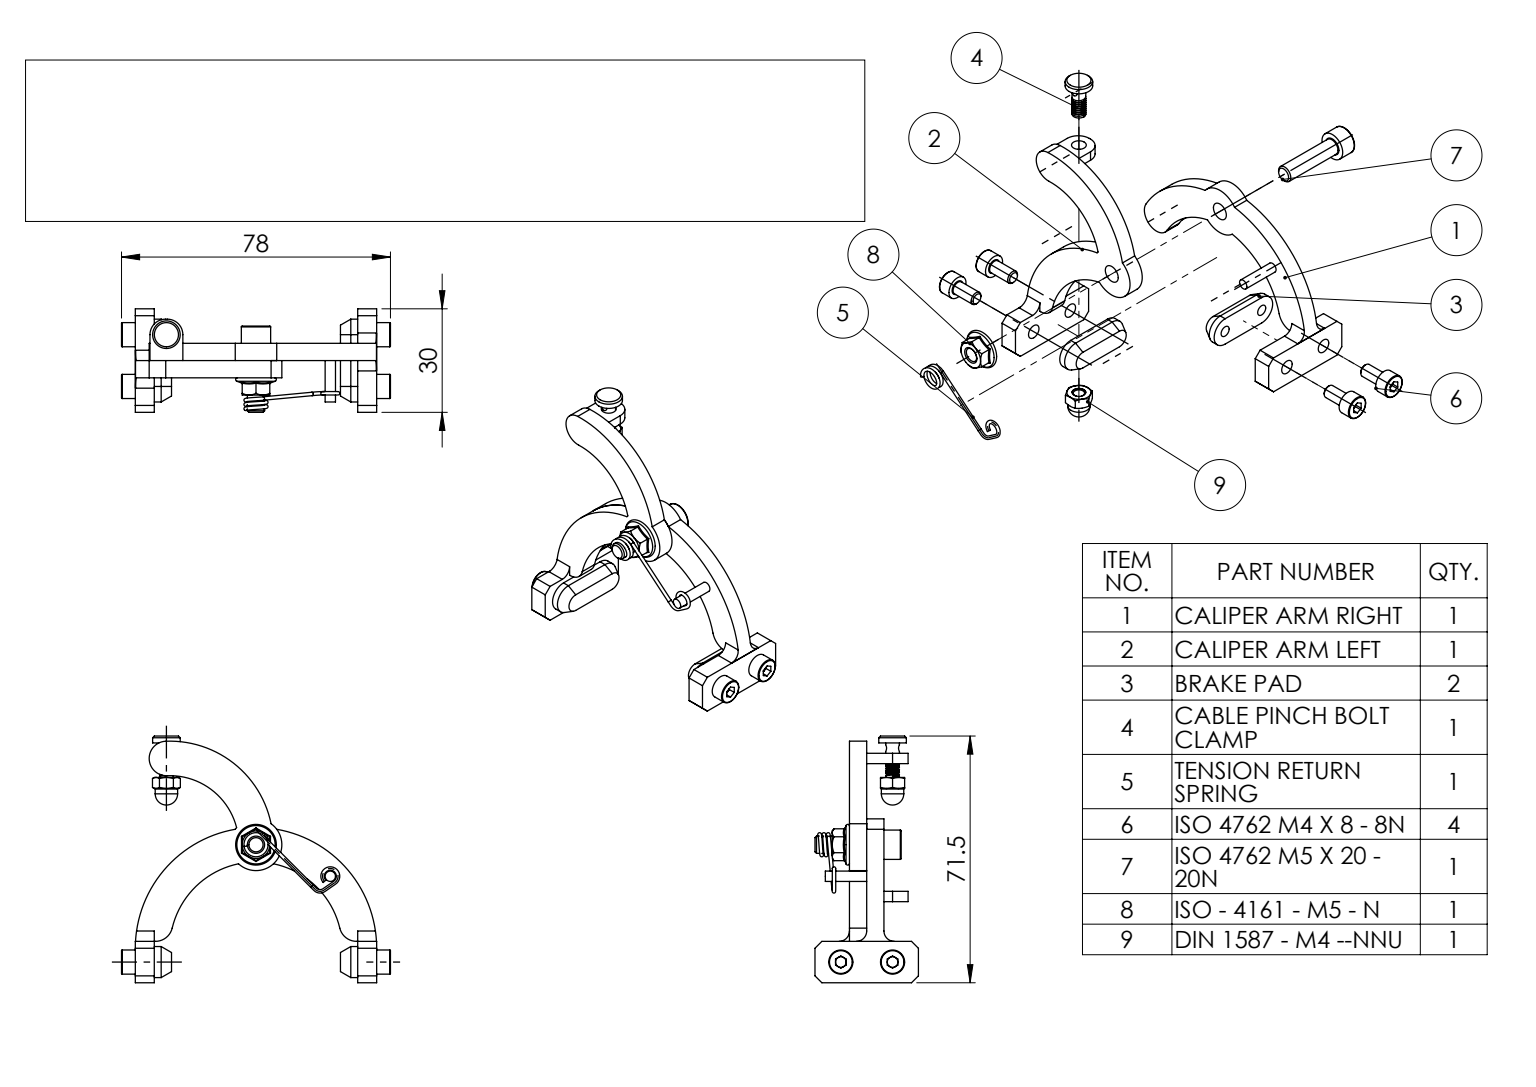
ISO-10303-21;
HEADER;
FILE_DESCRIPTION (('STEP AP214'),
    '1' );
FILE_NAME ('BR-590',
    '2026-10-08T05:45:04',
    ( '' ),
    ( '' ),
    'SwSTEP 2.0',
    'SolidWorks 2026',
    '' );
FILE_SCHEMA (( 'AUTOMOTIVE_DESIGN' ));
ENDSEC;

DATA;
#1 = CARTESIAN_POINT ( 'NONE',  ( 16.54959645279592451, 16.98593745313911896, 13.11591282735340336 ) ) ;
#2 =( LENGTH_UNIT ( ) NAMED_UNIT ( * ) SI_UNIT ( .MILLI., .METRE. ) );
#3 = CARTESIAN_POINT ( 'NONE',  ( 16.03488360228399046, 17.50065030364834939, 12.16198771834506509 ) ) ;
#4 = B_SPLINE_CURVE_WITH_KNOTS ( 'NONE', 3,
 ( #2921, #5637, #7133, #6355, #5528 ),
 .UNSPECIFIED., .F., .F.,
 ( 4, 1, 4 ),
 ( 5.640274452250024914E-20, 0.002309401076758505356, 0.004618802153517010713 ),
 .UNSPECIFIED. ) ;
#5 = CARTESIAN_POINT ( 'NONE',  ( 22.63806431670481700, 19.48506897666907989, 12.00579112326951758 ) ) ;
#6 = CARTESIAN_POINT ( 'NONE',  ( -25.98076211353311393, 52.34374999904395054, -3.128098921329806714 ) ) ;
#7 = CARTESIAN_POINT ( 'NONE',  ( -2.527408190673963162, 30.96936468028755840, 15.39281658473306358 ) ) ;
#8 = CARTESIAN_POINT ( 'NONE',  ( 3.200000000000000178, 2.020725942163657862, -3.499999999999999556 ) ) ;
#9 =( BOUNDED_CURVE ( )  B_SPLINE_CURVE ( 2, ( #10910, #4195, #7581, #6742, #4979, #7521, #70, #5149, #6620 ),
 .UNSPECIFIED., .F., .F. ) 
 B_SPLINE_CURVE_WITH_KNOTS ( ( 3, 2, 2, 2, 3 ),
 ( 0.6944444444444445308, 0.7037037037037037202, 0.7222222222222222099, 0.7407407407407406996, 0.7500000000000000000 ),
 .UNSPECIFIED. ) 
 CURVE ( )  GEOMETRIC_REPRESENTATION_ITEM ( )  RATIONAL_B_SPLINE_CURVE ( ( 0.9330127018922194093, 0.9330127018922197424, 1.000000000000000000, 0.8660254037844387076, 1.000000000000000000, 0.8660254037844387076, 1.000000000000000000, 0.9330127018922194093, 0.9330127018922194093 ) ) 
 REPRESENTATION_ITEM ( '' )  );
#10 = FACE_OUTER_BOUND ( 'NONE', #392, .T. ) ;
#11 = FACE_OUTER_BOUND ( 'NONE', #1428, .T. ) ;
#12 = VERTEX_POINT ( 'NONE', #2248 ) ;
#13 = ORIENTED_EDGE ( 'NONE', *, *, #10452, .T. ) ;
#14 = DIRECTION ( 'NONE',  ( 0.000000000000000000, 0.000000000000000000, 1.000000000000000000 ) ) ;
#15 = CONICAL_SURFACE ( 'NONE', #541, 4.000000000000000000, 0.8911886515913786111 ) ;
#16 = CARTESIAN_POINT ( 'NONE',  ( -4.211405944401398038, -2.460460786169389902, -3.751298493805494072 ) ) ;
#17 = CARTESIAN_POINT ( 'NONE',  ( 19.95755123817951215, 17.62047157401400810, 12.00579112326941988 ) ) ;
#18 = UNCERTAINTY_MEASURE_WITH_UNIT (LENGTH_MEASURE( 1.000000000000000082E-05 ), #5479, 'distance_accuracy_value', 'NONE');
#19 = CARTESIAN_POINT ( 'NONE',  ( -2.500000000000005329, 29.80321974748362734, 16.48359592357600789 ) ) ;
#20 = EDGE_CURVE ( 'NONE', #10326, #5059, #2301, .T. ) ;
#21 = LINE ( 'NONE', #8698, #9426 ) ;
#22 = CARTESIAN_POINT ( 'NONE',  ( -24.35964822603314417, 53.91874999904395338, -5.000000000000103029 ) ) ;
#23 = ADVANCED_FACE ( 'NONE', ( #9179, #3240, #3960 ), #10018, .T. ) ;
#24 = LINE ( 'NONE', #3426, #7602 ) ;
#25 = FACE_OUTER_BOUND ( 'NONE', #10724, .T. ) ;
#26 = CARTESIAN_POINT ( 'NONE',  ( 4.750000000000000888, 3.249999999999998668, 0.000000000000000000 ) ) ;
#27 = VECTOR ( 'NONE', #4855, 1000.000000000000000 ) ;
#28 = ORIENTED_EDGE ( 'NONE', *, *, #6003, .T. ) ;
#29 = DIRECTION ( 'NONE',  ( 6.098637220230963674E-17, -1.000000000000000000, 0.000000000000000000 ) ) ;
#30 = CARTESIAN_POINT ( 'NONE',  ( -25.98076211353311038, 60.99999999999985789, -0.9999999999995021760 ) ) ;
#31 = CARTESIAN_POINT ( 'NONE',  ( -24.35964822603314772, 52.63541666571061484, -4.064049460664953983 ) ) ;
#32 = CARTESIAN_POINT ( 'NONE',  ( -24.35964822603314772, 55.26041666571061484, -4.064049460664953983 ) ) ;
#33 = ADVANCED_FACE ( 'NONE', ( #727 ), #6680, .T. ) ;
#34 = CARTESIAN_POINT ( 'NONE',  ( 5.076455387921347651, 24.47916666666666075, -2.499999999999999112 ) ) ;
#35 = CARTESIAN_POINT ( 'NONE',  ( -26.98076211353309972, 53.23333333333319217, -6.732050807568954909 ) ) ;
#36 = AXIS2_PLACEMENT_3D ( 'NONE', #5242, #7853, #1848 ) ;
#37 = ORIENTED_EDGE ( 'NONE', *, *, #2342, .T. ) ;
#38 = VERTEX_POINT ( 'NONE', #5852 ) ;
#39 = CARTESIAN_POINT ( 'NONE',  ( 34.64101615137754209, 5.000000000000000888, 2.500000000000000000 ) ) ;
#40 = VERTEX_POINT ( 'NONE', #10965 ) ;
#41 = DIRECTION ( 'NONE',  ( 1.000000000000000000, 0.000000000000000000, 0.000000000000000000 ) ) ;
#42 = SURFACE_SIDE_STYLE ('',( #5116 ) ) ;
#43 = ORIENTED_EDGE ( 'NONE', *, *, #6494, .F. ) ;
#44 = CARTESIAN_POINT ( 'NONE',  ( 21.41951502703731691, 22.64547864373410135, 12.00579112326941988 ) ) ;
#45 = CARTESIAN_POINT ( 'NONE',  ( 2.449848172108560096, 3.432307619358740514, -3.503702292528905637 ) ) ;
#46 = CARTESIAN_POINT ( 'NONE',  ( 29.49999999999999289, -3.999999999999993339, 12.14999999999999503 ) ) ;
#47 = CARTESIAN_POINT ( 'NONE',  ( -25.17020516978313083, 50.01041666571061484, -6.403925809002825709 ) ) ;
#48 = CARTESIAN_POINT ( 'NONE',  ( 22.57450250028656669, 18.29201386669844709, 10.95195840513859231 ) ) ;
#49 = ADVANCED_FACE ( 'NONE', ( #5029 ), #6019, .T. ) ;
#50 = DIRECTION ( 'NONE',  ( 0.000000000000000000, 0.000000000000000000, -1.000000000000000000 ) ) ;
#51 = FACE_OUTER_BOUND ( 'NONE', #9561, .T. ) ;
#52 = CARTESIAN_POINT ( 'NONE',  ( -24.35964822603314417, 49.89374999904394770, -5.000000000000103029 ) ) ;
#53 = DIRECTION ( 'NONE',  ( 1.000000000000000000, 1.776356839400250465E-15, 0.000000000000000000 ) ) ;
#54 = ORIENTED_EDGE ( 'NONE', *, *, #4990, .T. ) ;
#55 = DIRECTION ( 'NONE',  ( -1.000000000000000000, 0.000000000000000000, 0.000000000000000000 ) ) ;
#56 = ORIENTED_EDGE ( 'NONE', *, *, #4099, .F. ) ;
#57 = CARTESIAN_POINT ( 'NONE',  ( 3.472591809326047052, 31.51591669395100936, 13.67406658473306535 ) ) ;
#58 = VERTEX_POINT ( 'NONE', #781 ) ;
#59 = CARTESIAN_POINT ( 'NONE',  ( 18.70477062293933557, 21.09978808922912208, 12.94889058896590583 ) ) ;
#60 = CARTESIAN_POINT ( 'NONE',  ( 16.65878245872646701, 16.87675144720473952, 12.10347664333366247 ) ) ;
#61 = CARTESIAN_POINT ( 'NONE',  ( 17.36588923991300604, 17.58385822839129986, 12.10347664333366247 ) ) ;
#62 = CARTESIAN_POINT ( 'NONE',  ( -26.79131905728310059, 52.28541666571062052, -3.596074190997381237 ) ) ;
#63 = CARTESIAN_POINT ( 'NONE',  ( -2.500000000000003997, 29.93383077435482065, 15.47094158473306535 ) ) ;
#64 = CARTESIAN_POINT ( 'NONE',  ( 0.1388410611045408360, -2.351840044243144856, 2.926493552095781325 ) ) ;
#65 = CARTESIAN_POINT ( 'NONE',  ( -26.85195975805010704, 58.50831236826149251, -6.801198016534330648 ) ) ;
#66 = ORIENTED_EDGE ( 'NONE', *, *, #10280, .F. ) ;
#67 = ORIENTED_EDGE ( 'NONE', *, *, #8603, .T. ) ;
#68 = AXIS2_PLACEMENT_3D ( 'NONE', #5659, #5549, #6578 ) ;
#69 = CARTESIAN_POINT ( 'NONE',  ( -2.688821387764050996E-14, -4.618802153517012954, -0.4999999999999995559 ) ) ;
#70 = CARTESIAN_POINT ( 'NONE',  ( -26.98076211353309972, 54.77916666475469754, -3.267949192431252037 ) ) ;
#71 = CARTESIAN_POINT ( 'NONE',  ( 19.29066956973784386, 17.16581860495888634, 12.00630190750973370 ) ) ;
#72 =( GEOMETRIC_REPRESENTATION_CONTEXT ( 3 ) GLOBAL_UNCERTAINTY_ASSIGNED_CONTEXT ( ( #3080 ) ) GLOBAL_UNIT_ASSIGNED_CONTEXT ( ( #8638, #7131, #1020 ) ) REPRESENTATION_CONTEXT ( 'NONE', 'WORKASPACE' ) );
#73 = EDGE_CURVE ( 'NONE', #9208, #2549, #8067, .T. ) ;
#74 = DIRECTION ( 'NONE',  ( 1.000000000000000000, 0.000000000000000000, 0.000000000000000000 ) ) ;
#75 = SHAPE_REPRESENTATION ( 'brake pad', ( #308 ), #6353 ) ;
#76 = CARTESIAN_POINT ( 'NONE',  ( 3.453038570460273071, 2.625189405340834448, -3.535263753543585352 ) ) ;
#77 = CARTESIAN_POINT ( 'NONE',  ( -25.98076211353311393, 55.49374999904395622, -6.871901078670400231 ) ) ;
#78 = VECTOR ( 'NONE', #4837, 1000.000000000000000 ) ;
#79 = DIRECTION ( 'NONE',  ( 0.000000000000000000, -1.000000000000000000, 0.000000000000000000 ) ) ;
#80 = CARTESIAN_POINT ( 'NONE',  ( 24.49999999999999289, -3.999999999999986233, -4.999999999999992006 ) ) ;
#81 = CARTESIAN_POINT ( 'NONE',  ( 29.50000000000000711, 1.387778780781445676E-14, -12.50000000000000000 ) ) ;
#82 = EDGE_LOOP ( 'NONE', ( #7039, #8451, #8267 ) ) ;
#83 = CIRCLE ( 'NONE', #1502, 3.500000000000000000 ) ;
#84 = LINE ( 'NONE', #3373, #8593 ) ;
#85 = CARTESIAN_POINT ( 'NONE',  ( -25.98076211353311393, 54.22499999999985931, -3.000000000000132339 ) ) ;
#86 = CIRCLE ( 'NONE', #6829, 2.149999999999992362 ) ;
#87 = ADVANCED_FACE ( 'NONE', ( #5248 ), #2694, .F. ) ;
#88 = CARTESIAN_POINT ( 'NONE',  ( -24.35964822603314417, 52.69374999904394485, -5.000000000000103029 ) ) ;
#89 = DIRECTION ( 'NONE',  ( 1.156482317317871478E-16, -0.000000000000000000, -1.000000000000000000 ) ) ;
#90 = EDGE_CURVE ( 'NONE', #5054, #1107, #1851, .T. ) ;
#91 = AXIS2_PLACEMENT_3D ( 'NONE', #3480, #6860, #2653 ) ;
#92 = CARTESIAN_POINT ( 'NONE',  ( 20.23853826540680600, 19.71164639310234534, 12.00579112326941988 ) ) ;
#93 = CARTESIAN_POINT ( 'NONE',  ( -27.98076211353308551, 54.69166666666652787, -6.154700538379338504 ) ) ;
#94 = AXIS2_PLACEMENT_3D ( 'NONE', #6317, #9708, #415 ) ;
#95 = ORIENTED_EDGE ( 'NONE', *, *, #9906, .F. ) ;
#96 = ORIENTED_EDGE ( 'NONE', *, *, #10897, .F. ) ;
#97 = DIRECTION ( 'NONE',  ( 1.000000000000000000, -0.000000000000000000, -0.000000000000000000 ) ) ;
#98 = EDGE_CURVE ( 'NONE', #7309, #1456, #9352, .T. ) ;
#99 = FACE_OUTER_BOUND ( 'NONE', #8308, .T. ) ;
#100 = AXIS2_PLACEMENT_3D ( 'NONE', #6064, #8518, #3293 ) ;
#101 = VERTEX_POINT ( 'NONE', #7634 ) ;
#102 = CARTESIAN_POINT ( 'NONE',  ( 21.21106610644839208, 53.49999999999983658, 14.50000000000000000 ) ) ;
#103 = CARTESIAN_POINT ( 'NONE',  ( 4.200000000000001954, 0.000000000000000000, 0.000000000000000000 ) ) ;
#104 = VECTOR ( 'NONE', #726, 999.9999999999998863 ) ;
#105 = CARTESIAN_POINT ( 'NONE',  ( 6.876213465810407786E-15, -3.202582148906756299, -1.452965002680407514 ) ) ;
#106 = CARTESIAN_POINT ( 'NONE',  ( -25.17020516978313083, 50.71041666571061057, -6.403925809002825709 ) ) ;
#107 = EDGE_CURVE ( 'NONE', #8667, #6915, #8632, .T. ) ;
#108 = EDGE_CURVE ( 'NONE', #2494, #2915, #8401, .T. ) ;
#109 = CARTESIAN_POINT ( 'NONE',  ( 16.61199375056689931, 16.92354015536430722, 11.10566822806672427 ) ) ;
#110 = CARTESIAN_POINT ( 'NONE',  ( 4.200000000000001954, 0.000000000000000000, 2.000000000000000888 ) ) ;
#111 = CARTESIAN_POINT ( 'NONE',  ( -27.60187600103308014, 50.88541666571062194, -5.935950539335252074 ) ) ;
#112 = CARTESIAN_POINT ( 'NONE',  ( 21.21106610644839208, 56.49999999999984368, 14.50000000000000000 ) ) ;
#113 = EDGE_LOOP ( 'NONE', ( #698, #4129, #8999, #2220 ) ) ;
#114 = CARTESIAN_POINT ( 'NONE',  ( -25.84804642293430277, 59.00000000000105871, -3.000000000000019984 ) ) ;
#115 = EDGE_LOOP ( 'NONE', ( #4415, #1242, #292 ) ) ;
#116 = CARTESIAN_POINT ( 'NONE',  ( -2.521662442312484931, 32.42808502599334730, 12.81469158473306713 ) ) ;
#117 = ORIENTED_EDGE ( 'NONE', *, *, #2558, .T. ) ;
#118 = CARTESIAN_POINT ( 'NONE',  ( 22.45649315185626094, 23.58010107951569623, 12.94889058896590583 ) ) ;
#119 = FILL_AREA_STYLE_COLOUR ( '', #3145 ) ;
#120 = EDGE_CURVE ( 'NONE', #1703, #4005, #3527, .T. ) ;
#121 = CARTESIAN_POINT ( 'NONE',  ( 19.90085419568980640, 16.36478119802090703, 11.95042571680015442 ) ) ;
#122 = CARTESIAN_POINT ( 'NONE',  ( 19.29066956973784386, 17.16581860495888634, 12.00630190750973370 ) ) ;
#123 = CARTESIAN_POINT ( 'NONE',  ( -26.79131905728310059, 50.65208333237728766, -6.403925809002825709 ) ) ;
#124 = CARTESIAN_POINT ( 'NONE',  ( 2.500000000000008438, 30.00000000000000711, 14.59375000000000178 ) ) ;
#125 = PRODUCT_DEFINITION_FORMATION_WITH_SPECIFIED_SOURCE ( 'ANY', '', #9165, .NOT_KNOWN. ) ;
#126 = DIRECTION ( 'NONE',  ( -4.029251166000348040E-16, -0.7071067811865463515, 0.7071067811865486830 ) ) ;
#127 = DIRECTION ( 'NONE',  ( 0.000000000000000000, 0.000000000000000000, 1.000000000000000000 ) ) ;
#128 = ORIENTED_EDGE ( 'NONE', *, *, #2197, .F. ) ;
#129 = EDGE_CURVE ( 'NONE', #9236, #8327, #4531, .T. ) ;
#130 = ORIENTED_EDGE ( 'NONE', *, *, #7314, .T. ) ;
#131 = EDGE_CURVE ( 'NONE', #6804, #8565, #10133, .T. ) ;
#132 = CARTESIAN_POINT ( 'NONE',  ( -30.75045812061784289, 13.49999999999941913, -5.000000000000000000 ) ) ;
#133 = DIRECTION ( 'NONE',  ( 0.000000000000000000, 1.000000000000000000, 0.000000000000000000 ) ) ;
#134 = CONICAL_SURFACE ( 'NONE', #6343, 1.610000000000000098, 0.7853981633974741472 ) ;
#135 = CONICAL_SURFACE ( 'NONE', #3683, 4.624785217660733139, 1.047197551196604071 ) ;
#136 = CARTESIAN_POINT ( 'NONE',  ( 23.04535143233503192, 19.92821688535955360, 12.00579112326941988 ) ) ;
#137 = CARTESIAN_POINT ( 'NONE',  ( -26.98076211353309972, 52.76666666666653072, -3.267949192431252037 ) ) ;
#138 = CARTESIAN_POINT ( 'NONE',  ( 0.6810597143197052450, 4.461075778259290914, -3.598441714920602053 ) ) ;
#139 = CARTESIAN_POINT ( 'NONE',  ( -24.35964822603314772, 54.56041666571061910, -4.064049460664953983 ) ) ;
#140 = DIRECTION ( 'NONE',  ( 0.7512361908166118596, 0.6577071706380241967, 0.05536662621717060306 ) ) ;
#141 = CARTESIAN_POINT ( 'NONE',  ( 0.000000000000000000, 0.000000000000000000, 0.000000000000000000 ) ) ;
#142 = CARTESIAN_POINT ( 'NONE',  ( 3.680118525130245732, -2.494084732383344605, -0.3507732604232533524 ) ) ;
#143 = VERTEX_POINT ( 'NONE', #4423 ) ;
#144 = CIRCLE ( 'NONE', #7774, 5.560781378645573980 ) ;
#145 = CARTESIAN_POINT ( 'NONE',  ( 1.101703131577913553, 32.47259180932605460, 17.07593341526694530 ) ) ;
#146 = ADVANCED_FACE ( 'NONE', ( #1748 ), #9290, .T. ) ;
#147 = PRESENTATION_LAYER_ASSIGNMENT (  '', '', ( #10621 ) ) ;
#148 = CARTESIAN_POINT ( 'NONE',  ( 2.500000000000007550, 31.03553390593274486, 14.67187500000000178 ) ) ;
#149 = CARTESIAN_POINT ( 'NONE',  ( -24.35964822603314417, 55.49374999904394912, -5.000000000000103029 ) ) ;
#150 = DIRECTION ( 'NONE',  ( -1.000000000000000000, -0.000000000000000000, -0.000000000000000000 ) ) ;
#151 = VECTOR ( 'NONE', #2662, 1000.000000000000000 ) ;
#152 = AXIS2_PLACEMENT_3D ( 'NONE', #3028, #4590, #5417 ) ;
#153 = FACE_OUTER_BOUND ( 'NONE', #113, .T. ) ;
#154 = CARTESIAN_POINT ( 'NONE',  ( -23.98076211353314235, 54.39999999999986358, -5.000000000000103029 ) ) ;
#155 = EDGE_LOOP ( 'NONE', ( #5166, #1454, #3473, #6221, #8889 ) ) ;
#156 = ORIENTED_EDGE ( 'NONE', *, *, #2088, .F. ) ;
#157 = DIRECTION ( 'NONE',  ( -1.000000000000000000, 0.000000000000000000, 0.000000000000000000 ) ) ;
#158 = EDGE_CURVE ( 'NONE', #2901, #3727, #5085, .T. ) ;
#159 = CARTESIAN_POINT ( 'NONE',  ( -4.000000000000000000, 0.000000000000000000, 0.000000000000000000 ) ) ;
#160 = PRODUCT_CONTEXT ( 'NONE', #1750, 'mechanical' ) ;
#161 = ORIENTED_EDGE ( 'NONE', *, *, #5009, .F. ) ;
#162 = CARTESIAN_POINT ( 'NONE',  ( -6.015568632492056977, 34.47916666666665009, 0.000000000000000000 ) ) ;
#163 = CARTESIAN_POINT ( 'NONE',  ( -23.98076211353314235, 54.34166666666652645, -3.845299461620867554 ) ) ;
#164 = CARTESIAN_POINT ( 'NONE',  ( 18.88912242859132107, 19.99746927611068870, 11.95042449705224819 ) ) ;
#165 = ADVANCED_FACE ( 'NONE', ( #10 ), #10244, .T. ) ;
#166 = CARTESIAN_POINT ( 'NONE',  ( -3.349226789952655547, -2.685125164760744809, -0.2236248678334863682 ) ) ;
#167 = ADVANCED_FACE ( 'NONE', ( #9404 ), #2582, .F. ) ;
#168 = CARTESIAN_POINT ( 'NONE',  ( -26.79131905728310059, 53.86041666571061626, -3.596074190997381237 ) ) ;
#169 = DIRECTION ( 'NONE',  ( -1.000000000000000000, 0.000000000000000000, 0.000000000000000000 ) ) ;
#170 = VERTEX_POINT ( 'NONE', #8523 ) ;
#171 = DIRECTION ( 'NONE',  ( 1.000000000000000000, 0.000000000000000000, 0.000000000000000000 ) ) ;
#172 = ORIENTED_EDGE ( 'NONE', *, *, #2907, .T. ) ;
#173 = CARTESIAN_POINT ( 'NONE',  ( -1.515916693951010252, 33.47259180932604750, 13.98656658473306713 ) ) ;
#174 = ORIENTED_EDGE ( 'NONE', *, *, #8829, .T. ) ;
#175 = CARTESIAN_POINT ( 'NONE',  ( 22.08651808663882932, 17.88512374315008557, 11.95042449705224819 ) ) ;
#176 = PRESENTATION_STYLE_ASSIGNMENT (( #8567 ) ) ;
#177 = CARTESIAN_POINT ( 'NONE',  ( 23.34652552892808330, 18.77429515943753202, 11.95042449705224819 ) ) ;
#178 = DIRECTION ( 'NONE',  ( -2.775557561562891351E-17, -1.000000000000000000, 8.326672684688671588E-17 ) ) ;
#179 = CARTESIAN_POINT ( 'NONE',  ( -26.79131905728310059, 52.05208333237728624, -6.403925809002825709 ) ) ;
#180 = CARTESIAN_POINT ( 'NONE',  ( 0.000000000000000000, 0.000000000000000000, -2.500000000000000000 ) ) ;
#181 = CARTESIAN_POINT ( 'NONE',  ( 4.750000000000000888, -1.622657008870242882E-15, 0.000000000000000000 ) ) ;
#182 = DIRECTION ( 'NONE',  ( 0.000000000000000000, -1.000000000000000000, 9.783878858594328898E-16 ) ) ;
#183 = VERTEX_POINT ( 'NONE', #900 ) ;
#184 = ORIENTED_EDGE ( 'NONE', *, *, #1115, .T. ) ;
#185 = FACE_OUTER_BOUND ( 'NONE', #10123, .T. ) ;
#186 = CARTESIAN_POINT ( 'NONE',  ( -25.98076211353311393, 49.49999999999986500, -5.000000000000103029 ) ) ;
#187 = FACE_OUTER_BOUND ( 'NONE', #10441, .T. ) ;
#188 = DIRECTION ( 'NONE',  ( 1.000000000000000000, 6.098637220230964906E-17, 0.000000000000000000 ) ) ;
#189 = CARTESIAN_POINT ( 'NONE',  ( -25.17020516978313083, 55.43541666571061910, -6.403925809002825709 ) ) ;
#190 = CYLINDRICAL_SURFACE ( 'NONE', #9308, 1.999999999999971356 ) ;
#191 = LINE ( 'NONE', #5261, #9329 ) ;
#192 = EDGE_CURVE ( 'NONE', #5966, #5040, #1802, .T. ) ;
#193 = ORIENTED_EDGE ( 'NONE', *, *, #720, .T. ) ;
#194 = FACE_OUTER_BOUND ( 'NONE', #2327, .T. ) ;
#195 = CIRCLE ( 'NONE', #3924, 7.500000000000000000 ) ;
#196 = CARTESIAN_POINT ( 'NONE',  ( -1.814555661125937247, 28.27902175519318817, 16.37280841526694175 ) ) ;
#197 = CARTESIAN_POINT ( 'NONE',  ( -2.500000000000005773, 29.99999999999999645, 13.96875000000000355 ) ) ;
#198 = UNCERTAINTY_MEASURE_WITH_UNIT (LENGTH_MEASURE( 1.000000000000000082E-05 ), #3270, 'distance_accuracy_value', 'NONE');
#199 = CARTESIAN_POINT ( 'NONE',  ( -26.98076211353408382, 57.99999999999985789, -6.732050807568389139 ) ) ;
#200 = CARTESIAN_POINT ( 'NONE',  ( -23.98076211353314235, 55.15833333333319644, -6.154700538379337615 ) ) ;
#201 = CARTESIAN_POINT ( 'NONE',  ( 0.000000000000000000, 3.980102097228895766E-16, -3.249999999999998224 ) ) ;
#202 = CARTESIAN_POINT ( 'NONE',  ( 34.99999999999987210, -7.999999999999996447, -12.50000000000000000 ) ) ;
#203 = EDGE_LOOP ( 'NONE', ( #3359, #5772 ) ) ;
#204 = ORIENTED_EDGE ( 'NONE', *, *, #3358, .T. ) ;
#205 = DIRECTION ( 'NONE',  ( 1.000000000000000000, 0.000000000000000000, 0.000000000000000000 ) ) ;
#206 = CARTESIAN_POINT ( 'NONE',  ( 2.000000000000000000, 0.000000000000000000, 0.000000000000000000 ) ) ;
#207 = CARTESIAN_POINT ( 'NONE',  ( 7.145701223178938965E-16, 30.00000000000000000, 12.50000000000000000 ) ) ;
#208 = ORIENTED_EDGE ( 'NONE', *, *, #385, .F. ) ;
#209 = LINE ( 'NONE', #6940, #5064 ) ;
#210 = DIRECTION ( 'NONE',  ( 0.000000000000000000, 1.000000000000000000, -1.345283343056720273E-15 ) ) ;
#211 = AXIS2_PLACEMENT_3D ( 'NONE', #8616, #9603, #2730 ) ;
#212 = CARTESIAN_POINT ( 'NONE',  ( 24.35722724902042202, 20.98982846826517346, 11.95042449705185739 ) ) ;
#213 = CARTESIAN_POINT ( 'NONE',  ( 3.500000000000007550, 28.55025253169416644, 15.76562500000000178 ) ) ;
#214 = CARTESIAN_POINT ( 'NONE',  ( -25.98076211353311393, 54.26874999904394059, -6.871901078670400231 ) ) ;
#215 = LINE ( 'NONE', #1106, #6427 ) ;
#216 = ORIENTED_EDGE ( 'NONE', *, *, #9478, .T. ) ;
#217 = LINE ( 'NONE', #1960, #6352 ) ;
#218 = PRODUCT ( 'brake pad', 'brake pad', '', ( #1890 ) ) ;
#219 = ORIENTED_EDGE ( 'NONE', *, *, #3408, .T. ) ;
#220 = CARTESIAN_POINT ( 'NONE',  ( -0.06616922564517661864, 33.50000000000000000, 12.65844158473306535 ) ) ;
#221 = CIRCLE ( 'NONE', #5903, 1.649999999999998579 ) ;
#222 = ORIENTED_EDGE ( 'NONE', *, *, #1600, .T. ) ;
#223 = CARTESIAN_POINT ( 'NONE',  ( 24.37916169550391032, 20.40431285142311424, 12.94889058896590761 ) ) ;
#224 = PRESENTATION_STYLE_ASSIGNMENT (( #9345 ) ) ;
#225 = EDGE_CURVE ( 'NONE', #3283, #7506, #8145, .T. ) ;
#226 = CARTESIAN_POINT ( 'NONE',  ( 18.76105380172462844, 21.09515122317004909, 11.95042449705224819 ) ) ;
#227 = ADVANCED_FACE ( 'NONE', ( #1969 ), #10407, .F. ) ;
#228 = FACE_OUTER_BOUND ( 'NONE', #3011, .T. ) ;
#229 = CARTESIAN_POINT ( 'NONE',  ( -26.79131905728310059, 51.58541666571061768, -3.596074190997381237 ) ) ;
#230 = CARTESIAN_POINT ( 'NONE',  ( 34.99999999999987210, 2.000000000000002220, -12.50000000000000000 ) ) ;
#231 = CARTESIAN_POINT ( 'NONE',  ( 34.99999999999999289, 2.000000000000002220, -12.49999999999999822 ) ) ;
#232 = FACE_OUTER_BOUND ( 'NONE', #6046, .T. ) ;
#233 = VERTEX_POINT ( 'NONE', #9571 ) ;
#234 = VERTEX_POINT ( 'NONE', #10467 ) ;
#235 = CARTESIAN_POINT ( 'NONE',  ( 16.74199038346592872, 18.20775708483950694, 12.16198771834549497 ) ) ;
#236 = EDGE_CURVE ( 'NONE', #3617, #2973, #5354, .T. ) ;
#237 = LINE ( 'NONE', #3635, #4176 ) ;
#238 = DIRECTION ( 'NONE',  ( 0.000000000000000000, 0.000000000000000000, 1.000000000000000000 ) ) ;
#239 = CARTESIAN_POINT ( 'NONE',  ( -27.44132740410865523, 55.89336612041927310, -4.296608737464627126 ) ) ;
#240 = CARTESIAN_POINT ( 'NONE',  ( 6.015568632492061418, 34.47916666666664298, -2.499999999999998668 ) ) ;
#241 = DIRECTION ( 'NONE',  ( 4.312387734421983755E-17, -0.7071067811865462405, -0.7071067811865489050 ) ) ;
#242 = EDGE_CURVE ( 'NONE', #1228, #6486, #8792, .T. ) ;
#243 = SURFACE_SIDE_STYLE ('',( #1130 ) ) ;
#244 = CARTESIAN_POINT ( 'NONE',  ( 1.449747468305833120, 33.50000000000000000, 16.07812500000000355 ) ) ;
#245 = CARTESIAN_POINT ( 'NONE',  ( 4.000000000000000000, -2.309401076758516691, -0.4999999999999995559 ) ) ;
#246 = AXIS2_PLACEMENT_3D ( 'NONE', #4153, #7547, #5055 ) ;
#247 = ORIENTED_EDGE ( 'NONE', *, *, #9284, .F. ) ;
#248 = DIRECTION ( 'NONE',  ( 0.000000000000000000, 0.000000000000000000, -1.000000000000000000 ) ) ;
#249 = CARTESIAN_POINT ( 'NONE',  ( -1.767766952966370209, 28.23223304703362402, 15.37500000000000355 ) ) ;
#250 = CARTESIAN_POINT ( 'NONE',  ( -2.500000000000005773, 29.99999999999999645, 16.46875000000000355 ) ) ;
#251 = CARTESIAN_POINT ( 'NONE',  ( -26.98076211353408382, 57.86742347890963600, -6.732050807568390027 ) ) ;
#252 = CONICAL_SURFACE ( 'NONE', #4877, 2.767949192431121919, 0.5235987755982963732 ) ;
#253 = EDGE_CURVE ( 'NONE', #7504, #6853, #3627, .T. ) ;
#254 = CARTESIAN_POINT ( 'NONE',  ( -25.98076211353324894, 16.50000000000026290, -7.149999999999990585 ) ) ;
#255 = DIRECTION ( 'NONE',  ( -1.000000000000000000, -0.000000000000000000, -0.000000000000000000 ) ) ;
#256 = CARTESIAN_POINT ( 'NONE',  ( -26.98076211353309972, 55.33333333333320070, -6.732050807568954909 ) ) ;
#257 = AXIS2_PLACEMENT_3D ( 'NONE', #5414, #5255, #8742 ) ;
#258 = EDGE_LOOP ( 'NONE', ( #649, #8272, #6684, #10787 ) ) ;
#259 = AXIS2_PLACEMENT_3D ( 'NONE', #6737, #6069, #4302 ) ;
#260 = CIRCLE ( 'NONE', #5589, 4.000000000000600409 ) ;
#261 = EDGE_LOOP ( 'NONE', ( #3712, #6126, #2093, #9383 ) ) ;
#262 = PLANE ( 'NONE',  #4144 ) ;
#263 = FACE_OUTER_BOUND ( 'NONE', #1330, .T. ) ;
#264 = SHAPE_DEFINITION_REPRESENTATION ( #5799, #7540 ) ;
#265 = EDGE_LOOP ( 'NONE', ( #1963, #2238, #5184, #1794 ) ) ;
#266 = DIRECTION ( 'NONE',  ( 0.000000000000000000, 0.8660254037844380415, -0.5000000000000012212 ) ) ;
#267 = VECTOR ( 'NONE', #7158, 1000.000000000000000 ) ;
#268 = DIRECTION ( 'NONE',  ( 0.000000000000000000, 0.000000000000000000, 1.000000000000000000 ) ) ;
#269 = VECTOR ( 'NONE', #6345, 1000.000000000000000 ) ;
#270 = VECTOR ( 'NONE', #9575, 1000.000000000000000 ) ;
#271 = CARTESIAN_POINT ( 'NONE',  ( 23.84774077504003031, 19.42364242282459230, 10.95195840513859231 ) ) ;
#272 = CARTESIAN_POINT ( 'NONE',  ( 2.474873734152918558, 32.47487373415292211, 16.00000000000000355 ) ) ;
#273 = CARTESIAN_POINT ( 'NONE',  ( -24.35964822603314772, 51.23541666571061626, -4.064049460664953983 ) ) ;
#274 = VECTOR ( 'NONE', #6744, 1000.000000000000000 ) ;
#275 = CARTESIAN_POINT ( 'NONE',  ( 2.500000000000000000, 0.000000000000000000, 0.000000000000000000 ) ) ;
#276 = VERTEX_POINT ( 'NONE', #6124 ) ;
#277 = LINE ( 'NONE', #2902, #2443 ) ;
#278 = ORIENTED_EDGE ( 'NONE', *, *, #1388, .F. ) ;
#279 = CARTESIAN_POINT ( 'NONE',  ( -1.814555661125939912, 31.72097824480680117, 15.31469158473306713 ) ) ;
#280 = VECTOR ( 'NONE', #7293, 1000.000000000000000 ) ;
#281 = VERTEX_POINT ( 'NONE', #1064 ) ;
#282 = ADVANCED_FACE ( 'NONE', ( #10574 ), #1338, .F. ) ;
#283 = CARTESIAN_POINT ( 'NONE',  ( 23.89484671925281845, 19.39402032390267649, 11.95042449705224819 ) ) ;
#284 = CARTESIAN_POINT ( 'NONE',  ( 0.000000000000000000, 30.00000000000000000, 2.500000000000000000 ) ) ;
#285 = CARTESIAN_POINT ( 'NONE',  ( 22.06757164964230711, 19.02077357123424406, 13.00425721518307576 ) ) ;
#287 = CARTESIAN_POINT ( 'NONE',  ( -27.60187600103308370, 55.66874999904394627, -5.000000000000103029 ) ) ;
#286 = AXIS2_PLACEMENT_3D ( 'NONE', #4193, #3362, #6741 ) ;
#288 = FACE_OUTER_BOUND ( 'NONE', #1831, .T. ) ;
#289 = PLANE ( 'NONE',  #436 ) ;
#290 = DIRECTION ( 'NONE',  ( 0.000000000000000000, 1.000000000000000000, 0.000000000000000000 ) ) ;
#291 = ADVANCED_FACE ( 'NONE', ( #6283 ), #7022, .T. ) ;
#292 = ORIENTED_EDGE ( 'NONE', *, *, #3597, .F. ) ;
#293 = EDGE_CURVE ( 'NONE', #9873, #5764, #10428, .T. ) ;
#294 = CARTESIAN_POINT ( 'NONE',  ( -27.78268512908116961, 55.49961679590672503, -4.132201955500060642 ) ) ;
#295 = PLANE ( 'NONE',  #9853 ) ;
#296 = PLANE ( 'NONE',  #4705 ) ;
#297 = LINE ( 'NONE', #1976, #5079 ) ;
#298 = AXIS2_PLACEMENT_3D ( 'NONE', #7550, #10165, #3387 ) ;
#299 = CARTESIAN_POINT ( 'NONE',  ( 2.000000000000000000, 0.8865213383406715941, 1.535499999999999199 ) ) ;
#300 = CARTESIAN_POINT ( 'NONE',  ( -1.515916693951006478, 26.52740819067394895, 16.45093341526693820 ) ) ;
#301 = CARTESIAN_POINT ( 'NONE',  ( 24.49999999999999289, -3.999999999999986233, -9.499999999999991118 ) ) ;
#302 = EDGE_CURVE ( 'NONE', #8162, #681, #1693, .T. ) ;
#303 = ORIENTED_EDGE ( 'NONE', *, *, #5009, .T. ) ;
#304 = LINE ( 'NONE', #1193, #3144 ) ;
#305 = EDGE_CURVE ( 'NONE', #10997, #8894, #7125, .T. ) ;
#306 = CARTESIAN_POINT ( 'NONE',  ( -2.500000000000007550, 30.06616922564517580, 14.96655841526694175 ) ) ;
#307 =( GEOMETRIC_REPRESENTATION_CONTEXT ( 3 ) GLOBAL_UNCERTAINTY_ASSIGNED_CONTEXT ( ( #7294 ) ) GLOBAL_UNIT_ASSIGNED_CONTEXT ( ( #5535, #3754, #8140 ) ) REPRESENTATION_CONTEXT ( 'NONE', 'WORKASPACE' ) );
#308 = AXIS2_PLACEMENT_3D ( 'NONE', #6956, #4296, #9565 ) ;
#309 = CARTESIAN_POINT ( 'NONE',  ( 4.197393957002303999, 7.772902908466098641E-14, -3.503767560748929810 ) ) ;
#310 = CARTESIAN_POINT ( 'NONE',  ( 19.29066956973784386, 17.16581860495888634, 12.00630190750973370 ) ) ;
#311 = CARTESIAN_POINT ( 'NONE',  ( -24.98076211353313170, 54.89583333142136468, -3.267949192431250705 ) ) ;
#312 = DIRECTION ( 'NONE',  ( -0.000000000000000000, 1.000000000000000000, -0.000000000000000000 ) ) ;
#313 = CARTESIAN_POINT ( 'NONE',  ( -25.98076211353311393, 54.26874999904394059, -6.871901078670400231 ) ) ;
#314 = CARTESIAN_POINT ( 'NONE',  ( 27.50000000000001066, 0.5000000000000162093, 10.00000000000000888 ) ) ;
#315 = AXIS2_PLACEMENT_3D ( 'NONE', #3172, #7503, #4003 ) ;
#316 = CARTESIAN_POINT ( 'NONE',  ( 0.000000000000000000, 0.000000000000000000, -4.484454397937119197 ) ) ;
#317 = EDGE_LOOP ( 'NONE', ( #5235, #5389 ) ) ;
#318 = VERTEX_POINT ( 'NONE', #2131 ) ;
#319 = FACE_OUTER_BOUND ( 'NONE', #5879, .T. ) ;
#320 = CARTESIAN_POINT ( 'NONE',  ( 34.99999999999987210, -3.999999999999989786, 7.850000000000003197 ) ) ;
#321 = APPLICATION_PROTOCOL_DEFINITION ( 'draft international standard', 'automotive_design', 1998, #10976 ) ;
#322 = ORIENTED_EDGE ( 'NONE', *, *, #302, .T. ) ;
#323 = VECTOR ( 'NONE', #3846, 1000.000000000000114 ) ;
#324 = CARTESIAN_POINT ( 'NONE',  ( -2.000000000000002665, -3.464101615137770374, -3.142992957459237680 ) ) ;
#325 = CARTESIAN_POINT ( 'NONE',  ( -25.98076211353310683, 49.89374999904395480, -6.871901078670399343 ) ) ;
#326 = CIRCLE ( 'NONE', #6705, 2.649999999999991029 ) ;
#327 = CARTESIAN_POINT ( 'NONE',  ( 19.66613420429507997, 17.48520406133187066, 11.00732503135576401 ) ) ;
#328 = ORIENTED_EDGE ( 'NONE', *, *, #9673, .F. ) ;
#329 = CARTESIAN_POINT ( 'NONE',  ( -27.60187600103308370, 53.04374999904394627, -5.000000000000103029 ) ) ;
#330 = ORIENTED_EDGE ( 'NONE', *, *, #4103, .T. ) ;
#331 = CARTESIAN_POINT ( 'NONE',  ( -21.21106610644865498, 16.50000000000026290, -9.500000000000000000 ) ) ;
#332 = ORIENTED_EDGE ( 'NONE', *, *, #981, .F. ) ;
#333 = CARTESIAN_POINT ( 'NONE',  ( -2.500000000000007550, 31.03553390593274486, 13.89062500000000355 ) ) ;
#334 = ORIENTED_EDGE ( 'NONE', *, *, #9479, .T. ) ;
#335 = CARTESIAN_POINT ( 'NONE',  ( 24.30080945327229003, 20.98731269034403368, 10.95195840513820151 ) ) ;
#336 = FILL_AREA_STYLE ('',( #9671 ) ) ;
#337 = CARTESIAN_POINT ( 'NONE',  ( 19.48730207459019326, 19.05393922246431870, 11.95042449705224996 ) ) ;
#338 = CARTESIAN_POINT ( 'NONE',  ( 16.95349311633468403, 16.58206632678699677, 13.07803561935715742 ) ) ;
#339 = CARTESIAN_POINT ( 'NONE',  ( -25.98076211353311393, 54.44374999904394485, -3.128098921329806714 ) ) ;
#340 = CARTESIAN_POINT ( 'NONE',  ( 2.000000000000000000, 1.773042676681340524, -2.059984127722458425E-15 ) ) ;
#341 = CARTESIAN_POINT ( 'NONE',  ( -25.44486372867087454, 53.05623925897106830, -7.000000000000073719 ) ) ;
#342 = ORIENTED_EDGE ( 'NONE', *, *, #1250, .F. ) ;
#343 = ORIENTED_EDGE ( 'NONE', *, *, #9950, .F. ) ;
#344 = CARTESIAN_POINT ( 'NONE',  ( 0.2949799022107380542, 1.977804580622975611E-16, -1.615000000000000213 ) ) ;
#345 = CARTESIAN_POINT ( 'NONE',  ( 0.2704726383733979667, 0.000000000000000000, 0.000000000000000000 ) ) ;
#346 = CARTESIAN_POINT ( 'NONE',  ( -25.98076211353324894, 14.99999999999984190, -2.500000000000000000 ) ) ;
#347 = DIRECTION ( 'NONE',  ( 0.000000000000000000, 1.000000000000000000, -1.471414886128461471E-15 ) ) ;
#348 = CARTESIAN_POINT ( 'NONE',  ( -21.21106610644865498, 13.49999999999941913, -5.000000000000000000 ) ) ;
#349 = CARTESIAN_POINT ( 'NONE',  ( 0.000000000000000000, 0.000000000000000000, 0.000000000000000000 ) ) ;
#350 = CARTESIAN_POINT ( 'NONE',  ( 20.05579831881754060, 20.86490736922957367, 14.50000000000000000 ) ) ;
#351 = CARTESIAN_POINT ( 'NONE',  ( -2.521662442312484931, 32.42808502599334730, 12.81469158473306713 ) ) ;
#352 = CARTESIAN_POINT ( 'NONE',  ( 0.1999999999999987899, 0.000000000000000000, 3.500000000000000000 ) ) ;
#353 = ORIENTED_EDGE ( 'NONE', *, *, #8457, .F. ) ;
#354 = CARTESIAN_POINT ( 'NONE',  ( 2.472591809326055046, 28.89829686842209355, 16.76343341526694175 ) ) ;
#355 = DIRECTION ( 'NONE',  ( -6.098637220230966139E-17, 1.000000000000000000, 0.000000000000000000 ) ) ;
#356 = FACE_OUTER_BOUND ( 'NONE', #2898, .T. ) ;
#357 = CARTESIAN_POINT ( 'NONE',  ( -26.85338401696505883, 57.49468158336109269, -6.800474515642543238 ) ) ;
#358 = EDGE_CURVE ( 'NONE', #6966, #10495, #2017, .T. ) ;
#359 = FACE_OUTER_BOUND ( 'NONE', #4823, .T. ) ;
#360 = ADVANCED_FACE ( 'NONE', ( #8018 ), #2971, .F. ) ;
#361 = CARTESIAN_POINT ( 'NONE',  ( 34.99999999999999289, -3.999999999999993339, 10.00000000000000533 ) ) ;
#362 = CARTESIAN_POINT ( 'NONE',  ( -26.79131905728310059, 52.92708333237727913, -6.403925809002825709 ) ) ;
#363 = DIRECTION ( 'NONE',  ( 0.000000000000000000, 0.000000000000000000, -1.000000000000000000 ) ) ;
#364 = DIRECTION ( 'NONE',  ( 6.098637220230964906E-17, -1.000000000000000000, 0.000000000000000000 ) ) ;
#365 = ORIENTED_EDGE ( 'NONE', *, *, #5871, .F. ) ;
#366 = ORIENTED_EDGE ( 'NONE', *, *, #5633, .F. ) ;
#367 = CARTESIAN_POINT ( 'NONE',  ( -25.98076211353310683, 54.92499999999986926, -3.000000000000132339 ) ) ;
#368 = DIRECTION ( 'NONE',  ( 0.000000000000000000, 0.000000000000000000, -1.000000000000000000 ) ) ;
#369 = CONTEXT_DEPENDENT_SHAPE_REPRESENTATION ( #4008, #1822 ) ;
#370 = ORIENTED_EDGE ( 'NONE', *, *, #1853, .F. ) ;
#371 = CARTESIAN_POINT ( 'NONE',  ( 25.98076211353311749, 53.49999999999983658, 10.00000000000000178 ) ) ;
#372 = EDGE_CURVE ( 'NONE', #1417, #4847, #7538, .T. ) ;
#373 = AXIS2_PLACEMENT_3D ( 'NONE', #9911, #4914, #9286 ) ;
#374 = CYLINDRICAL_SURFACE ( 'NONE', #7364, 7.500000000000000000 ) ;
#375 = CARTESIAN_POINT ( 'NONE',  ( 22.78377297911024257, 19.69285065907503807, 11.00732503135576401 ) ) ;
#376 = ORIENTED_EDGE ( 'NONE', *, *, #1216, .F. ) ;
#377 = ADVANCED_FACE ( 'NONE', ( #7914 ), #289, .T. ) ;
#378 = CARTESIAN_POINT ( 'NONE',  ( -24.35964822603314772, 54.73541666571060915, -4.064049460664953983 ) ) ;
#379 = ORIENTED_EDGE ( 'NONE', *, *, #4517, .F. ) ;
#380 = DIRECTION ( 'NONE',  ( 0.000000000000000000, 0.000000000000000000, 1.000000000000000000 ) ) ;
#381 = VERTEX_POINT ( 'NONE', #2236 ) ;
#382 = CARTESIAN_POINT ( 'NONE',  ( -2.500000000000004441, 28.96446609406725159, 14.04687500000000355 ) ) ;
#383 = ORIENTED_EDGE ( 'NONE', *, *, #9617, .T. ) ;
#384 = CARTESIAN_POINT ( 'NONE',  ( 16.45601903647678910, 17.07951486945825792, 11.12029599681952519 ) ) ;
#385 = EDGE_CURVE ( 'NONE', #9319, #2915, #3021, .T. ) ;
#386 = CARTESIAN_POINT ( 'NONE',  ( 4.000000000000000000, 0.000000000000000000, 0.000000000000000000 ) ) ;
#387 = CARTESIAN_POINT ( 'NONE',  ( 18.14679736200770677, 17.01284808935846371, 13.04404649446423115 ) ) ;
#388 = CARTESIAN_POINT ( 'NONE',  ( -27.98076211353308551, 49.84999999999986642, -5.000000000000103029 ) ) ;
#389 = AXIS2_PLACEMENT_3D ( 'NONE', #8545, #5873, #9257 ) ;
#390 = DIRECTION ( 'NONE',  ( 1.000000000000000000, 0.000000000000000000, 0.000000000000000000 ) ) ;
#391 = DIRECTION ( 'NONE',  ( 4.312387734422005941E-17, -0.7071067811865500152, 0.7071067811865451302 ) ) ;
#392 = EDGE_LOOP ( 'NONE', ( #6819, #3302, #6878, #5552 ) ) ;
#393 = ORIENTED_EDGE ( 'NONE', *, *, #3763, .T. ) ;
#394 = CARTESIAN_POINT ( 'NONE',  ( 23.17052989764754756, 21.62756661655841839, 12.00579112326981246 ) ) ;
#395 = DIRECTION ( 'NONE',  ( 0.000000000000000000, 0.000000000000000000, -1.000000000000000000 ) ) ;
#396 = PRODUCT_DEFINITION_SHAPE ( 'NONE', 'NONE',  #11006 ) ;
#397 = DIRECTION ( 'NONE',  ( -1.000000000000000000, -0.000000000000000000, -0.000000000000000000 ) ) ;
#398 = DIRECTION ( 'NONE',  ( -4.312387734421998546E-17, 0.7071067811865489050, -0.7071067811865462405 ) ) ;
#399 = CARTESIAN_POINT ( 'NONE',  ( -25.98076211353311393, 55.88749999808803182, -7.000000000000072831 ) ) ;
#400 = DIRECTION ( 'NONE',  ( -1.000000000000000000, -0.000000000000000000, -0.000000000000000000 ) ) ;
#401 =( LENGTH_UNIT ( ) NAMED_UNIT ( * ) SI_UNIT ( .MILLI., .METRE. ) );
#402 = CARTESIAN_POINT ( 'NONE',  ( -0.06616922564517119243, 26.49999999999999289, 16.52905841526693820 ) ) ;
#403 = CARTESIAN_POINT ( 'NONE',  ( 4.800000000000000711, 2.020667218593132755E-16, -1.649999999999999911 ) ) ;
#404 = ORIENTED_EDGE ( 'NONE', *, *, #1797, .F. ) ;
#405 = DIRECTION ( 'NONE',  ( -0.000000000000000000, -0.000000000000000000, -1.000000000000000000 ) ) ;
#406 = CARTESIAN_POINT ( 'NONE',  ( -3.472591809326048384, 31.51591669395100936, 14.88843341526694353 ) ) ;
#407 = CARTESIAN_POINT ( 'NONE',  ( -1.515916693951006478, 26.52740819067394895, 15.20093341526694353 ) ) ;
#408 = LINE ( 'NONE', #8607, #638 ) ;
#409 = EDGE_CURVE ( 'NONE', #4738, #10440, #8087, .T. ) ;
#410 = DIRECTION ( 'NONE',  ( 1.000000000000000000, 0.000000000000000000, 0.000000000000000000 ) ) ;
#411 = CARTESIAN_POINT ( 'NONE',  ( 4.000000000000003553, 0.000000000000000000, 3.500000000000000000 ) ) ;
#412 = CARTESIAN_POINT ( 'NONE',  ( -4.236525694536558362, 2.416953475386465211, -3.751298745799836354 ) ) ;
#413 = CARTESIAN_POINT ( 'NONE',  ( -24.35964822603314417, 52.69374999904394485, -5.000000000000103029 ) ) ;
#414 = FACE_OUTER_BOUND ( 'NONE', #5327, .T. ) ;
#415 = DIRECTION ( 'NONE',  ( 0.000000000000000000, 0.4999999999999993894, -0.8660254037844389297 ) ) ;
#416 = ORIENTED_EDGE ( 'NONE', *, *, #2889, .T. ) ;
#417 = CARTESIAN_POINT ( 'NONE',  ( -1.312671235360383548, -3.860931062424228788, -0.05923475698271369466 ) ) ;
#418 = EDGE_CURVE ( 'NONE', #6185, #829, #4717, .T. ) ;
#419 = EDGE_LOOP ( 'NONE', ( #2323, #566, #3009, #4097 ) ) ;
#420 = VECTOR ( 'NONE', #4987, 1000.000000000000000 ) ;
#421 = EDGE_CURVE ( 'NONE', #10496, #6333, #10386, .T. ) ;
#422 = PLANE ( 'NONE',  #6643 ) ;
#423 = DIRECTION ( 'NONE',  ( 1.000000000000000000, 0.000000000000000000, 0.000000000000000000 ) ) ;
#424 = CIRCLE ( 'NONE', #2569, 0.5000000000000013323 ) ;
#425 = CARTESIAN_POINT ( 'NONE',  ( 23.19605965318632457, 18.72439211931539660, 10.95195840513869179 ) ) ;
#426 = AXIS2_PLACEMENT_3D ( 'NONE', #206, #8665, #6156 ) ;
#427 = ORIENTED_EDGE ( 'NONE', *, *, #10489, .T. ) ;
#428 = CARTESIAN_POINT ( 'NONE',  ( 2.887392608830845031, -2.020725942164465661, -3.499999999999999556 ) ) ;
#429 = EDGE_CURVE ( 'NONE', #7102, #2953, #8173, .T. ) ;
#430 = B_SPLINE_CURVE_WITH_KNOTS ( 'NONE', 3,
 ( #3945, #1448, #2175, #4061, #499, #4743 ),
 .UNSPECIFIED., .F., .F.,
 ( 4, 2, 4 ),
 ( 0.000000000000000000, 0.0002095117440854730670, 0.0004190234881709461339 ),
 .UNSPECIFIED. ) ;
#431 = ORIENTED_EDGE ( 'NONE', *, *, #9265, .T. ) ;
#432 = CARTESIAN_POINT ( 'NONE',  ( 0.1381424733900992741, -1.355358988605521287, 3.500000000000000000 ) ) ;
#433 = VERTEX_POINT ( 'NONE', #9014 ) ;
#434 = CARTESIAN_POINT ( 'NONE',  ( -0.06616922564517727090, 32.50000000000000711, 15.15844158473306535 ) ) ;
#435 = ORIENTED_EDGE ( 'NONE', *, *, #8120, .F. ) ;
#436 = AXIS2_PLACEMENT_3D ( 'NONE', #3684, #4797, #8278 ) ;
#437 = CARTESIAN_POINT ( 'NONE',  ( 21.34610222965416071, 23.60463303817794412, 10.95195840513859231 ) ) ;
#438 = AXIS2_PLACEMENT_3D ( 'NONE', #345, #1017, #4528 ) ;
#439 = CIRCLE ( 'NONE', #9129, 7.500000000000000000 ) ;
#440 = ADVANCED_FACE ( 'NONE', ( #7446 ), #6442, .F. ) ;
#441 = EDGE_CURVE ( 'NONE', #38, #9170, #10272, .T. ) ;
#442 = CARTESIAN_POINT ( 'NONE',  ( 0.1381424733901099877, -1.355358988605575687, -3.500000000000000000 ) ) ;
#443 = CARTESIAN_POINT ( 'NONE',  ( 19.16668011427331919, 17.04844365417888596, 13.00677669558776550 ) ) ;
#444 = VECTOR ( 'NONE', #10181, 1000.000000000000000 ) ;
#445 = CARTESIAN_POINT ( 'NONE',  ( -4.024497503033519941, 2.323544716729375459, -3.572167766733379768 ) ) ;
#446 = AXIS2_PLACEMENT_3D ( 'NONE', #473, #2203, #364 ) ;
#447 = DIRECTION ( 'NONE',  ( 0.000000000000000000, 0.000000000000000000, -1.000000000000000000 ) ) ;
#448 = FACE_BOUND ( 'NONE', #1109, .T. ) ;
#449 = EDGE_LOOP ( 'NONE', ( #1165, #1039, #7351, #5920, #1589 ) ) ;
#450 = ORIENTED_EDGE ( 'NONE', *, *, #5486, .T. ) ;
#451 = CARTESIAN_POINT ( 'NONE',  ( 21.51635413324704160, 18.70478684647606826, 12.00579112326941988 ) ) ;
#452 = DIRECTION ( 'NONE',  ( 0.000000000000000000, 0.000000000000000000, -1.000000000000000000 ) ) ;
#453 = CARTESIAN_POINT ( 'NONE',  ( -25.44486372867087454, 52.44373926088289295, -7.000000000000073719 ) ) ;
#454 = CARTESIAN_POINT ( 'NONE',  ( 24.99999259214812142, 30.01924558493218598, 2.500000000000000000 ) ) ;
#455 = CARTESIAN_POINT ( 'NONE',  ( -25.47388223254686324, 57.12817616725342162, -6.938581062208108108 ) ) ;
#457 = EDGE_CURVE ( 'NONE', #3885, #9988, #8075, .T. ) ;
#456 = DIRECTION ( 'NONE',  ( 0.000000000000000000, -1.000000000000000000, 1.287488025362403787E-15 ) ) ;
#458 = CARTESIAN_POINT ( 'NONE',  ( -3.500000000000003553, 31.44974746830583356, 16.39062500000000355 ) ) ;
#459 = LINE ( 'NONE', #9638, #280 ) ;
#460 = EDGE_CURVE ( 'NONE', #7106, #9208, #10799, .T. ) ;
#461 = ORIENTED_EDGE ( 'NONE', *, *, #4163, .T. ) ;
#462 = CARTESIAN_POINT ( 'NONE',  ( 0.000000000000000000, 0.000000000000000000, 0.000000000000000000 ) ) ;
#463 = CIRCLE ( 'NONE', #817, 2.041999999999999815 ) ;
#464 = CARTESIAN_POINT ( 'NONE',  ( -0.06616922564517033201, 27.49999999999998934, 15.27905841526694175 ) ) ;
#465 = CARTESIAN_POINT ( 'NONE',  ( 27.50000000000001066, -8.499999999999985789, -4.999999999999992006 ) ) ;
#466 = PRODUCT ( 'socket head cap screw_iso_ISO 4762 M5 x 20 - 20N', 'socket head cap screw_iso_ISO 4762 M5 x 20 - 20N', '', ( #3718 ) ) ;
#467 = CARTESIAN_POINT ( 'NONE',  ( -25.44486372867087809, 52.35623925897106545, -7.000000000000075495 ) ) ;
#468 = CARTESIAN_POINT ( 'NONE',  ( -25.71106610644865498, 13.49999999999941913, -5.000000000000000000 ) ) ;
#469 = CARTESIAN_POINT ( 'NONE',  ( -23.98076211353314235, 51.54166666666652219, -3.845299461620867554 ) ) ;
#470 = CARTESIAN_POINT ( 'NONE',  ( -24.35964822603314417, 53.39374999904394770, -5.000000000000103029 ) ) ;
#471 = B_SPLINE_CURVE_WITH_KNOTS ( 'NONE', 3,
 ( #1292, #9621, #2745, #445, #3626, #7912 ),
 .UNSPECIFIED., .F., .F.,
 ( 4, 2, 4 ),
 ( -3.640115492410698714E-06, 0.0002066546034006521879, 0.0004169493222937151081 ),
 .UNSPECIFIED. ) ;
#472 = LINE ( 'NONE', #3971, #9797 ) ;
#473 = CARTESIAN_POINT ( 'NONE',  ( -3.049318610115482207E-16, 5.000000000000000000, -5.500000000000000000 ) ) ;
#474 = ORIENTED_EDGE ( 'NONE', *, *, #7144, .T. ) ;
#475 = VECTOR ( 'NONE', #4688, 1000.000000000000000 ) ;
#476 = COLOUR_RGB ( '', 0.09019608, 0.27058824, 0.51372549) ;
#477 = DIRECTION ( 'NONE',  ( -1.000000000000000000, -0.000000000000000000, -0.000000000000000000 ) ) ;
#478 = DIRECTION ( 'NONE',  ( 0.000000000000000000, 0.000000000000000000, -1.000000000000000000 ) ) ;
#479 = EDGE_LOOP ( 'NONE', ( #4396, #7220, #4636, #9662 ) ) ;
#480 = DIRECTION ( 'NONE',  ( 0.000000000000000000, 0.000000000000000000, 1.000000000000000000 ) ) ;
#481 =( BOUNDED_CURVE ( )  B_SPLINE_CURVE ( 3, ( #678, #7459, #10848, #6612 ),
 .UNSPECIFIED., .F., .F. ) 
 B_SPLINE_CURVE_WITH_KNOTS ( ( 4, 4 ),
 ( 0.001563228649568143037, 0.003126104531729810565 ),
 .UNSPECIFIED. ) 
 CURVE ( )  GEOMETRIC_REPRESENTATION_ITEM ( )  RATIONAL_B_SPLINE_CURVE ( ( 1.000000000000000888, 0.3333333333333335369, 0.3333333333333327042, 1.000000000000000000 ) ) 
 REPRESENTATION_ITEM ( '' )  );
#482 = CARTESIAN_POINT ( 'NONE',  ( -25.98076211353310683, 51.29374999904394627, -6.871901078670399343 ) ) ;
#483 = AXIS2_PLACEMENT_3D ( 'NONE', #5841, #2237, #5628 ) ;
#484 = AXIS2_PLACEMENT_3D ( 'NONE', #7051, #937, #5776 ) ;
#485 = CARTESIAN_POINT ( 'NONE',  ( 21.34610222965416071, 23.60463303817794412, 10.95195840513859231 ) ) ;
#486 = EDGE_LOOP ( 'NONE', ( #10969, #5668, #5395 ) ) ;
#487 = CARTESIAN_POINT ( 'NONE',  ( -31.74999999999995737, 0.000000000000000000, 0.000000000000000000 ) ) ;
#488 = ADVANCED_FACE ( 'NONE', ( #4064 ), #713, .F. ) ;
#489 = ORIENTED_EDGE ( 'NONE', *, *, #920, .T. ) ;
#490 = CARTESIAN_POINT ( 'NONE',  ( -1.391697335622809950, -4.043246145443391448, -3.503898532754372575 ) ) ;
#491 = VERTEX_POINT ( 'NONE', #504 ) ;
#492 = AXIS2_PLACEMENT_3D ( 'NONE', #4378, #1817, #4149 ) ;
#493 = PLANE ( 'NONE',  #6999 ) ;
#494 = SURFACE_STYLE_USAGE ( .BOTH. , #3060 ) ;
#495 = ORIENTED_EDGE ( 'NONE', *, *, #3771, .F. ) ;
#496 = AXIS2_PLACEMENT_3D ( 'NONE', #9924, #9081, #4871 ) ;
#497 = CARTESIAN_POINT ( 'NONE',  ( 16.37803167940877458, 17.15750222652490820, 11.12760988119559258 ) ) ;
#498 = EDGE_CURVE ( 'NONE', #8162, #10935, #5839, .T. ) ;
#499 = CARTESIAN_POINT ( 'NONE',  ( 4.154306624731137099, 2.398490048084935822, -3.721999068284414847 ) ) ;
#500 = EDGE_CURVE ( 'NONE', #2280, #1840, #8424, .T. ) ;
#501 = PRESENTATION_LAYER_ASSIGNMENT (  '', '', ( #5307 ) ) ;
#502 = CARTESIAN_POINT ( 'NONE',  ( 22.73223279825284848, 19.49146071982302075, 13.00425721518307753 ) ) ;
#503 = CARTESIAN_POINT ( 'NONE',  ( -27.98076211353308551, 51.80416666475470322, -6.154700538379338504 ) ) ;
#504 = CARTESIAN_POINT ( 'NONE',  ( -25.98076211353311393, 51.77499999999986358, -7.000000000000072831 ) ) ;
#505 = CARTESIAN_POINT ( 'NONE',  ( 2.650000000000095834, 30.00000000000000000, -2.500000000000000000 ) ) ;
#506 = ORIENTED_EDGE ( 'NONE', *, *, #5067, .T. ) ;
#507 = EDGE_LOOP ( 'NONE', ( #5439, #6866, #1397, #7624 ) ) ;
#508 = CARTESIAN_POINT ( 'NONE',  ( 21.90605485701305000, 18.97586566459109392, 12.00579112326941988 ) ) ;
#509 = LINE ( 'NONE', #4853, #3476 ) ;
#510 = DIRECTION ( 'NONE',  ( 1.000000000000000000, 0.000000000000000000, 0.000000000000000000 ) ) ;
#511 = CARTESIAN_POINT ( 'NONE',  ( -27.98076211353308551, 52.50416666475469896, -6.154700538379338504 ) ) ;
#512 = LINE ( 'NONE', #2245, #1941 ) ;
#513 = CARTESIAN_POINT ( 'NONE',  ( 3.527408190673962274, 28.61642175733934934, 14.76781658473306535 ) ) ;
#514 = DIRECTION ( 'NONE',  ( 0.000000000000000000, 0.5000000000000011102, 0.8660254037844380415 ) ) ;
#515 = UNCERTAINTY_MEASURE_WITH_UNIT (LENGTH_MEASURE( 1.000000000000000082E-05 ), #7040, 'distance_accuracy_value', 'NONE');
#516 = VERTEX_POINT ( 'NONE', #9391 ) ;
#517 = DIRECTION ( 'NONE',  ( 0.000000000000000000, 0.000000000000000000, 1.000000000000000000 ) ) ;
#518 = CARTESIAN_POINT ( 'NONE',  ( -3.500000000000005329, 30.06616922564516869, 16.21655841526694175 ) ) ;
#519 = CARTESIAN_POINT ( 'NONE',  ( -25.98076211353324894, 13.49999999999941913, -7.149999999999990585 ) ) ;
#520 = CARTESIAN_POINT ( 'NONE',  ( 2.887392608830372964, -2.020725942163647648, 3.499999999999999556 ) ) ;
#521 = CARTESIAN_POINT ( 'NONE',  ( 25.00000000000000000, 0.000000000000000000, 0.000000000000000000 ) ) ;
#522 = CARTESIAN_POINT ( 'NONE',  ( -25.98076211353311393, 51.07499999999986784, -7.000000000000073719 ) ) ;
#523 = CARTESIAN_POINT ( 'NONE',  ( -24.35964822603314772, 54.03541666571061342, -4.064049460664953983 ) ) ;
#524 = EDGE_CURVE ( 'NONE', #2763, #4729, #7658, .T. ) ;
#525 = CARTESIAN_POINT ( 'NONE',  ( -25.98076211353311393, 49.49999999999986500, -3.000000000000131894 ) ) ;
#526 = LINE ( 'NONE', #9765, #6655 ) ;
#527 = EDGE_LOOP ( 'NONE', ( #10460, #8210, #7795, #10548 ) ) ;
#528 = CARTESIAN_POINT ( 'NONE',  ( 0.000000000000000000, 0.000000000000000000, -2.500000000000000000 ) ) ;
#529 = DIRECTION ( 'NONE',  ( 1.000000000000000000, 0.000000000000000000, 0.000000000000000000 ) ) ;
#530 = APPLICATION_CONTEXT ( 'automotive_design' ) ;
#531 = EDGE_LOOP ( 'NONE', ( #5767, #5211, #193 ) ) ;
#532 = CARTESIAN_POINT ( 'NONE',  ( 3.200000000000000178, 2.020725942163657862, -3.499999999999999556 ) ) ;
#533 = CARTESIAN_POINT ( 'NONE',  ( -25.17020516978313083, 51.70208333237728482, -3.596074190997380349 ) ) ;
#534 = CARTESIAN_POINT ( 'NONE',  ( 22.29575558078030895, 19.24694448270711788, 12.00579112326941988 ) ) ;
#535 = ORIENTED_EDGE ( 'NONE', *, *, #3962, .F. ) ;
#536 = CARTESIAN_POINT ( 'NONE',  ( -26.51666049839535688, 53.81876073720500386, -7.000000000000071942 ) ) ;
#537 = EDGE_LOOP ( 'NONE', ( #10892, #4237 ) ) ;
#538 = CARTESIAN_POINT ( 'NONE',  ( -6.473970235329672780E-16, -4.862606272033106691, -3.745885042887442395 ) ) ;
#539 = ORIENTED_EDGE ( 'NONE', *, *, #3211, .F. ) ;
#540 = CARTESIAN_POINT ( 'NONE',  ( 1.767766952966377314, 28.23223304703363112, 15.68750000000000355 ) ) ;
#541 = AXIS2_PLACEMENT_3D ( 'NONE', #3800, #8078, #5529 ) ;
#542 = ORIENTED_EDGE ( 'NONE', *, *, #9273, .T. ) ;
#543 =( BOUNDED_CURVE ( )  B_SPLINE_CURVE ( 2, ( #6474, #4774, #10656, #2205, #3047, #6421, #9819, #9874, #2732 ),
 .UNSPECIFIED., .F., .F. ) 
 B_SPLINE_CURVE_WITH_KNOTS ( ( 3, 2, 2, 2, 3 ),
 ( 0.6388888888888889506, 0.6481481481481481399, 0.6666666666666666297, 0.6851851851851852304, 0.6944444444444445308 ),
 .UNSPECIFIED. ) 
 CURVE ( )  GEOMETRIC_REPRESENTATION_ITEM ( )  RATIONAL_B_SPLINE_CURVE ( ( 0.9330127018922194093, 0.9330127018922197424, 1.000000000000000000, 0.8660254037844387076, 1.000000000000000000, 0.8660254037844387076, 1.000000000000000000, 0.9330127018922189652, 0.9330127018922194093 ) ) 
 REPRESENTATION_ITEM ( '' )  );
#544 = CARTESIAN_POINT ( 'NONE',  ( 20.23629815768686768, 16.66554095800588797, 10.95195840513859231 ) ) ;
#545 = ADVANCED_FACE ( 'NONE', ( #10947 ), #7561, .T. ) ;
#546 = CARTESIAN_POINT ( 'NONE',  ( 22.63773560303409127, 18.20111046790825782, 12.94889058896590583 ) ) ;
#547 = VECTOR ( 'NONE', #5638, 1000.000000000000114 ) ;
#548 = CARTESIAN_POINT ( 'NONE',  ( -23.98076211353314235, 50.81249999808803608, -5.000000000000103029 ) ) ;
#549 = CARTESIAN_POINT ( 'NONE',  ( 2.000000000000000000, 1.773042676681340524, -2.059984127722458425E-15 ) ) ;
#550 = CARTESIAN_POINT ( 'NONE',  ( -27.44132332507749794, 55.71836679508493262, -4.296600267573891685 ) ) ;
#551 = ORIENTED_EDGE ( 'NONE', *, *, #3434, .F. ) ;
#552 = EDGE_LOOP ( 'NONE', ( #3265, #5644 ) ) ;
#553 = EDGE_CURVE ( 'NONE', #10440, #6171, #9641, .T. ) ;
#554 = CARTESIAN_POINT ( 'NONE',  ( 20.47715220320264962, 17.98190999816754498, 12.00579112326941988 ) ) ;
#555 = EDGE_CURVE ( 'NONE', #6915, #590, #2328, .T. ) ;
#556 = FACE_OUTER_BOUND ( 'NONE', #1467, .T. ) ;
#557 = CARTESIAN_POINT ( 'NONE',  ( -6.259644161404862988E-16, -4.618802153517027165, -3.504271511726793076 ) ) ;
#558 = AXIS2_PLACEMENT_3D ( 'NONE', #4552, #8823, #7936 ) ;
#559 = LINE ( 'NONE', #7512, #10322 ) ;
#560 = CARTESIAN_POINT ( 'NONE',  ( 4.000000000000000000, 0.9868501483902631932, -0.09357334158579604100 ) ) ;
#561 = CARTESIAN_POINT ( 'NONE',  ( 1.814555661125942132, 28.27902175519319883, 13.43969158473306713 ) ) ;
#562 = CARTESIAN_POINT ( 'NONE',  ( -1.747541505913277282, 3.837784562140256650, -3.503702292528906526 ) ) ;
#563 = EDGE_LOOP ( 'NONE', ( #7565, #8832, #8917, #5557 ) ) ;
#564 = DIRECTION ( 'NONE',  ( -1.000000000000000000, 0.000000000000000000, 0.000000000000000000 ) ) ;
#565 = ADVANCED_FACE ( 'NONE', ( #10231 ), #7677, .T. ) ;
#566 = ORIENTED_EDGE ( 'NONE', *, *, #2127, .T. ) ;
#567 = CARTESIAN_POINT ( 'NONE',  ( -2.479565268636987785, 29.67421718125152452, 17.49702953738633937 ) ) ;
#568 = AXIS2_PLACEMENT_3D ( 'NONE', #528, #9502, #169 ) ;
#569 = DIRECTION ( 'NONE',  ( 0.000000000000000000, 1.000000000000000000, 0.000000000000000000 ) ) ;
#570 = LINE ( 'NONE', #9920, #2381 ) ;
#571 = CARTESIAN_POINT ( 'NONE',  ( -1.035533905932736420, 27.49999999999998934, 14.20312500000000355 ) ) ;
#572 = EDGE_CURVE ( 'NONE', #1489, #6302, #6943, .T. ) ;
#573 = EDGE_CURVE ( 'NONE', #652, #6838, #3756, .T. ) ;
#574 = CARTESIAN_POINT ( 'NONE',  ( -24.35964822603314417, 51.81874999904395196, -5.000000000000103029 ) ) ;
#575 = FACE_OUTER_BOUND ( 'NONE', #2113, .T. ) ;
#576 = CARTESIAN_POINT ( 'NONE',  ( 30.75045812061784289, 53.49999999999983658, 14.50000000000000000 ) ) ;
#577 = ORIENTED_EDGE ( 'NONE', *, *, #9425, .T. ) ;
#578 = CARTESIAN_POINT ( 'NONE',  ( -2.474873734152920335, 32.47487373415291501, 15.06250000000000355 ) ) ;
#579 = CARTESIAN_POINT ( 'NONE',  ( -2.000000000000007550, -3.464101615137749945, 0.000000000000000000 ) ) ;
#580 = CONTEXT_DEPENDENT_SHAPE_REPRESENTATION ( #3450, #9447 ) ;
#581 = ADVANCED_FACE ( 'NONE', ( #765 ), #3396, .T. ) ;
#582 = B_SPLINE_CURVE_WITH_KNOTS ( 'NONE', 3,
 ( #6456, #10019, #1519, #4189 ),
 .UNSPECIFIED., .F., .F.,
 ( 4, 4 ),
 ( 2.380739282169293681E-07, 0.002044882221487522803 ),
 .UNSPECIFIED. ) ;
#583 = CARTESIAN_POINT ( 'NONE',  ( -27.60187600103308725, 50.18541666571061199, -5.935950539335252074 ) ) ;
#584 = CARTESIAN_POINT ( 'NONE',  ( -27.60187600103308370, 54.26874999904394770, -5.000000000000103029 ) ) ;
#585 = CARTESIAN_POINT ( 'NONE',  ( 19.84380896203909828, 21.37294244821887546, 12.00579112326902731 ) ) ;
#586 = CARTESIAN_POINT ( 'NONE',  ( -26.98076211353309972, 49.96666666666652645, -3.267949192431252037 ) ) ;
#587 = ORIENTED_EDGE ( 'NONE', *, *, #9063, .T. ) ;
#588 = CARTESIAN_POINT ( 'NONE',  ( 3.199999999999999734, -3.031088913245550298, -1.749999999999972911 ) ) ;
#589 = ADVANCED_FACE ( 'NONE', ( #5232 ), #5948, .F. ) ;
#590 = VERTEX_POINT ( 'NONE', #5013 ) ;
#591 = AXIS2_PLACEMENT_3D ( 'NONE', #4501, #3714, #7053 ) ;
#592 = ORIENTED_EDGE ( 'NONE', *, *, #9149, .T. ) ;
#593 = LINE ( 'NONE', #3109, #5602 ) ;
#594 = EDGE_LOOP ( 'NONE', ( #6389, #7026, #1992, #1296 ) ) ;
#595 = CARTESIAN_POINT ( 'NONE',  ( 4.553649124439118623E-15, 27.49999999999999289, 15.53125000000000355 ) ) ;
#596 = ORIENTED_EDGE ( 'NONE', *, *, #6379, .F. ) ;
#597 = CARTESIAN_POINT ( 'NONE',  ( 17.60432978939287452, 17.35624782240900288, 11.07951759511215606 ) ) ;
#598 = PRESENTATION_STYLE_ASSIGNMENT (( #4897 ) ) ;
#599 = AXIS2_PLACEMENT_3D ( 'NONE', #2316, #6635, #3978 ) ;
#600 = VECTOR ( 'NONE', #4787, 1000.000000000000000 ) ;
#601 = CARTESIAN_POINT ( 'NONE',  ( -4.235164736271498614E-18, -0.3416191432522799887, -3.499999999999999556 ) ) ;
#602 = CARTESIAN_POINT ( 'NONE',  ( 19.75845051886964043, 23.09045650430892849, 12.94889058896590583 ) ) ;
#603 = EDGE_CURVE ( 'NONE', #9227, #143, #8788, .T. ) ;
#604 = CARTESIAN_POINT ( 'NONE',  ( -25.98076211353311393, 52.03749999808803040, -2.690598923241634743 ) ) ;
#605 = CIRCLE ( 'NONE', #5598, 4.499999999999999112 ) ;
#606 = CARTESIAN_POINT ( 'NONE',  ( 34.82492259089467979, 3.500278077966951340, -2.894288569839198022 ) ) ;
#607 = LINE ( 'NONE', #3224, #5645 ) ;
#608 = ADVANCED_FACE ( 'NONE', ( #7733 ), #3443, .T. ) ;
#609 = VERTEX_POINT ( 'NONE', #8450 ) ;
#610 = CARTESIAN_POINT ( 'NONE',  ( -1.515916693951006478, 26.52740819067394895, 16.45093341526693820 ) ) ;
#611 = AXIS2_PLACEMENT_3D ( 'NONE', #141, #10257, #7591 ) ;
#612 = ORIENTED_EDGE ( 'NONE', *, *, #2110, .F. ) ;
#613 = CARTESIAN_POINT ( 'NONE',  ( 19.55162244606592381, 17.33808635661342024, 12.00579012602852735 ) ) ;
#614 = CONICAL_SURFACE ( 'NONE', #2233, 2.055000000000000160, 0.7853981633974721488 ) ;
#615 = CARTESIAN_POINT ( 'NONE',  ( -25.44486372867087454, 52.15626073911682425, -3.000000000000131450 ) ) ;
#616 = DIRECTION ( 'NONE',  ( 1.000000000000000000, -0.000000000000000000, -0.000000000000000000 ) ) ;
#618 = CARTESIAN_POINT ( 'NONE',  ( 34.99999999999999289, 2.000000000000002220, 15.50000000000000533 ) ) ;
#617 = CONICAL_SURFACE ( 'NONE', #6842, 4.624785217660733139, 1.047197551196604071 ) ;
#619 = CARTESIAN_POINT ( 'NONE',  ( -3.472591809326043499, 28.48408330604899064, 14.29906658473306358 ) ) ;
#620 = CARTESIAN_POINT ( 'NONE',  ( -5.384454397937118664, 6.594054843588581554E-16, -4.484454397937119197 ) ) ;
#621 = ORIENTED_EDGE ( 'NONE', *, *, #5333, .T. ) ;
#622 = DIRECTION ( 'NONE',  ( -6.098637220230964906E-17, 1.000000000000000000, 0.000000000000000000 ) ) ;
#623 = EDGE_CURVE ( 'NONE', #6258, #6815, #9271, .T. ) ;
#624 = EDGE_CURVE ( 'NONE', #7008, #1215, #7866, .T. ) ;
#625 = VERTEX_POINT ( 'NONE', #5340 ) ;
#626 = CIRCLE ( 'NONE', #6313, 1.650000000000000355 ) ;
#627 = CARTESIAN_POINT ( 'NONE',  ( -3.500000000000005329, 30.06616922564516869, 14.96655841526694175 ) ) ;
#628 = AXIS2_PLACEMENT_3D ( 'NONE', #1690, #8407, #6856 ) ;
#629 = FACE_OUTER_BOUND ( 'NONE', #9860, .T. ) ;
#630 = DIRECTION ( 'NONE',  ( -1.000000000000000000, -0.000000000000000000, -0.000000000000000000 ) ) ;
#631 = CARTESIAN_POINT ( 'NONE',  ( 29.49999999999999289, 2.000000000000001776, 17.50000000000000000 ) ) ;
#632 = EDGE_CURVE ( 'NONE', #10983, #10935, #3603, .T. ) ;
#633 = DIRECTION ( 'NONE',  ( 1.000000000000000000, -0.000000000000000000, -0.000000000000000000 ) ) ;
#634 = CARTESIAN_POINT ( 'NONE',  ( -24.35964822603314772, 50.36041666571061626, -4.064049460664953983 ) ) ;
#635 = EDGE_CURVE ( 'NONE', #1703, #7385, #9558, .T. ) ;
#636 = CARTESIAN_POINT ( 'NONE',  ( -6.473970235329672780E-16, -4.862606272033106691, -3.745885042887442395 ) ) ;
#637 = DIRECTION ( 'NONE',  ( -1.000000000000000000, -0.000000000000000000, -0.000000000000000000 ) ) ;
#638 = VECTOR ( 'NONE', #3810, 1000.000000000000000 ) ;
#639 = ORIENTED_EDGE ( 'NONE', *, *, #10746, .T. ) ;
#640 = CARTESIAN_POINT ( 'NONE',  ( 1.449747468305836673, 26.49999999999999289, 14.35937500000000533 ) ) ;
#641 = CARTESIAN_POINT ( 'NONE',  ( 2.000000000000000000, 1.329782007511004727, -0.7677500000000018199 ) ) ;
#642 = CARTESIAN_POINT ( 'NONE',  ( -24.35964822603314772, 49.95208333237727771, -5.935950539335252074 ) ) ;
#643 = CARTESIAN_POINT ( 'NONE',  ( -27.60187600103308725, 51.52708333237728766, -4.064049460664955760 ) ) ;
#644 = CARTESIAN_POINT ( 'NONE',  ( 19.35452611835372849, 17.20101589911864437, 12.00579185514580338 ) ) ;
#645 = PRESENTATION_LAYER_ASSIGNMENT (  '', '', ( #2799 ) ) ;
#646 = CARTESIAN_POINT ( 'NONE',  ( -27.60187600103308370, 54.96874999904395054, -5.000000000000103029 ) ) ;
#647 = VERTEX_POINT ( 'NONE', #7310 ) ;
#648 = CARTESIAN_POINT ( 'NONE',  ( -27.60187600103308370, 55.14374999904394059, -5.000000000000103029 ) ) ;
#649 = ORIENTED_EDGE ( 'NONE', *, *, #10640, .T. ) ;
#650 = EDGE_LOOP ( 'NONE', ( #9124, #3568, #718, #1775 ) ) ;
#651 = DIRECTION ( 'NONE',  ( 0.000000000000000000, 0.000000000000000000, -1.000000000000000000 ) ) ;
#652 = VERTEX_POINT ( 'NONE', #7794 ) ;
#653 = DIRECTION ( 'NONE',  ( 1.000000000000000000, -0.000000000000000000, 1.156482317317871478E-16 ) ) ;
#654 = DIRECTION ( 'NONE',  ( 1.000000000000000000, 0.000000000000000000, 0.000000000000000000 ) ) ;
#655 = ORIENTED_EDGE ( 'NONE', *, *, #2585, .T. ) ;
#657 = CARTESIAN_POINT ( 'NONE',  ( 20.21677217982034946, 21.95921345637081501, 11.00732503135595941 ) ) ;
#656 = AXIS2_PLACEMENT_3D ( 'NONE', #1363, #6196, #4761 ) ;
#658 = CIRCLE ( 'NONE', #9718, 3.000000000000000000 ) ;
#659 = CARTESIAN_POINT ( 'NONE',  ( 0.000000000000000000, 30.00000000000000000, -2.499999999999998668 ) ) ;
#660 = CARTESIAN_POINT ( 'NONE',  ( -4.211140560182196957, -2.431303136016552013, -3.745885042887436178 ) ) ;
#661 = CARTESIAN_POINT ( 'NONE',  ( 22.11813463801259161, 17.83967204375498383, 12.94889058896590583 ) ) ;
#662 = CARTESIAN_POINT ( 'NONE',  ( -24.98076211353313170, 50.69583333142136183, -3.267949192431250705 ) ) ;
#663 = AXIS2_PLACEMENT_3D ( 'NONE', #9560, #2957, #1054 ) ;
#664 = DIRECTION ( 'NONE',  ( 1.000000000000000000, 0.000000000000000000, 0.000000000000000000 ) ) ;
#665 = CARTESIAN_POINT ( 'NONE',  ( 3.199999999999999734, 0.000000000000000000, -3.499999999999999556 ) ) ;
#666 = PRODUCT_DEFINITION_CONTEXT ( 'detailed design', #7209, 'design' ) ;
#667 = ORIENTED_EDGE ( 'NONE', *, *, #6516, .T. ) ;
#668 = VECTOR ( 'NONE', #8809, 1000.000000000000114 ) ;
#669 = CARTESIAN_POINT ( 'NONE',  ( -1.720978244806810498, 31.81455566112594013, 17.31030841526694175 ) ) ;
#670 = VERTEX_POINT ( 'NONE', #1318 ) ;
#671 = CARTESIAN_POINT ( 'NONE',  ( 19.95752144772427528, 19.94857296576799754, 13.00425721518131184 ) ) ;
#672 = VECTOR ( 'NONE', #10406, 1000.000000000000000 ) ;
#673 = DIRECTION ( 'NONE',  ( 0.000000000000000000, 0.000000000000000000, -1.000000000000000000 ) ) ;
#674 = VECTOR ( 'NONE', #5477, 1000.000000000000000 ) ;
#675 = CARTESIAN_POINT ( 'NONE',  ( 25.49999999999999645, -3.999999999999986233, -6.649999999999990585 ) ) ;
#676 = CARTESIAN_POINT ( 'NONE',  ( -0.3208286057739654917, 4.433571671609680465, -0.3503314178412548774 ) ) ;
#677 = CARTESIAN_POINT ( 'NONE',  ( -3.500000000000001332, 29.93383077435482065, 12.97094158473306358 ) ) ;
#678 = CARTESIAN_POINT ( 'NONE',  ( 15.87890888817147150, 17.65662501776163040, 12.17661548709639341 ) ) ;
#679 = ORIENTED_EDGE ( 'NONE', *, *, #9149, .F. ) ;
#680 = DIRECTION ( 'NONE',  ( -0.000000000000000000, -0.000000000000000000, -1.000000000000000000 ) ) ;
#681 = VERTEX_POINT ( 'NONE', #6948 ) ;
#682 = CARTESIAN_POINT ( 'NONE',  ( -26.51666049839536043, 52.09373926088289863, -3.000000000000133671 ) ) ;
#683 = LINE ( 'NONE', #4766, #3461 ) ;
#684 = PLANE ( 'NONE',  #6651 ) ;
#685 = EDGE_CURVE ( 'NONE', #8160, #10068, #10693, .T. ) ;
#686 = LINE ( 'NONE', #7469, #1983 ) ;
#687 = CARTESIAN_POINT ( 'NONE',  ( -24.35964822603314772, 54.73541666571060915, -4.064049460664953983 ) ) ;
#688 = CARTESIAN_POINT ( 'NONE',  ( 1.144235203016666258, 3.958177651039090250, -0.09382832055445661235 ) ) ;
#689 = CARTESIAN_POINT ( 'NONE',  ( 4.000000000000000000, -2.471525695159793035, -3.686886880705770864 ) ) ;
#690 = EDGE_LOOP ( 'NONE', ( #9028, #6042, #6525, #4019, #7005, #10810 ) ) ;
#691 = DIRECTION ( 'NONE',  ( -1.000000000000000000, -6.098637220230964906E-17, -0.000000000000000000 ) ) ;
#692 = CARTESIAN_POINT ( 'NONE',  ( -1.767766952966375094, 31.76776695296636888, 13.81250000000000355 ) ) ;
#693 = EDGE_CURVE ( 'NONE', #4635, #7216, #8152, .T. ) ;
#694 = CARTESIAN_POINT ( 'NONE',  ( -25.98076211353310683, 51.46874999904394343, -6.871901078670399343 ) ) ;
#695 = CARTESIAN_POINT ( 'NONE',  ( -26.79131905728310059, 53.68541666571061910, -3.596074190997381237 ) ) ;
#696 = CARTESIAN_POINT ( 'NONE',  ( 17.79249663040192431, 17.21067465782413919, 12.06642298039558980 ) ) ;
#697 = CARTESIAN_POINT ( 'NONE',  ( -25.98076211353311393, 52.47499999999985931, -7.309401076758571314 ) ) ;
#698 = ORIENTED_EDGE ( 'NONE', *, *, #108, .F. ) ;
#699 = ORIENTED_EDGE ( 'NONE', *, *, #1713, .T. ) ;
#700 = ORIENTED_EDGE ( 'NONE', *, *, #8785, .F. ) ;
#701 = PLANE ( 'NONE',  #10710 ) ;
#702 = VERTEX_POINT ( 'NONE', #6220 ) ;
#703 = EDGE_CURVE ( 'NONE', #3324, #4732, #543, .T. ) ;
#704 = CARTESIAN_POINT ( 'NONE',  ( -1.035533905932736420, 27.49999999999998934, 15.45312500000000178 ) ) ;
#705 = ORIENTED_EDGE ( 'NONE', *, *, #5043, .F. ) ;
#706 = CARTESIAN_POINT ( 'NONE',  ( 17.20991452582289583, 17.73983294248524700, 12.11810441208646338 ) ) ;
#707 = CARTESIAN_POINT ( 'NONE',  ( 27.50000000000001066, -3.999999999999986233, -4.999999999999992006 ) ) ;
#708 = CARTESIAN_POINT ( 'NONE',  ( 2.550604951803072673, 0.000000000000000000, 0.000000000000000000 ) ) ;
#709 = ADVANCED_FACE ( 'NONE', ( #6106 ), #741, .T. ) ;
#710 = CARTESIAN_POINT ( 'NONE',  ( 19.07396262421655919, 19.44200532275891291, 12.94889058896472811 ) ) ;
#711 = CARTESIAN_POINT ( 'NONE',  ( -25.98076211353311393, 53.78749999808803750, -7.309401076758571314 ) ) ;
#712 = AXIS2_PLACEMENT_3D ( 'NONE', #9244, #9413, #4259 ) ;
#713 = PLANE ( 'NONE',  #1157 ) ;
#714 = CARTESIAN_POINT ( 'NONE',  ( 3.060260095956253146, 1.362955318038518771, -3.500000000000000000 ) ) ;
#715 = ORIENTED_EDGE ( 'NONE', *, *, #7861, .T. ) ;
#716 = SHAPE_REPRESENTATION ( 'Tension Return Spring', ( #308 ), #3340 ) ;
#717 = CARTESIAN_POINT ( 'NONE',  ( 2.521662442312485819, 32.42808502599335441, 14.49780841526694175 ) ) ;
#718 = ORIENTED_EDGE ( 'NONE', *, *, #9054, .T. ) ;
#719 = CARTESIAN_POINT ( 'NONE',  ( 24.08125446323534291, 19.61299372598402613, 12.94889058896590761 ) ) ;
#720 = EDGE_CURVE ( 'NONE', #2294, #2160, #221, .T. ) ;
#721 = VECTOR ( 'NONE', #4124, 1000.000000000000000 ) ;
#722 = CARTESIAN_POINT ( 'NONE',  ( 2.000000000000000000, 0.8865213383406680414, -1.535500000000000975 ) ) ;
#723 = DIRECTION ( 'NONE',  ( 1.000000000000000000, 0.000000000000000000, 0.000000000000000000 ) ) ;
#724 = LINE ( 'NONE', #7457, #721 ) ;
#725 = CARTESIAN_POINT ( 'NONE',  ( -2.500000000000003997, 29.93383077435482065, 14.22094158473306535 ) ) ;
#726 = DIRECTION ( 'NONE',  ( -0.8191520442889875797, 1.003171929053519570E-16, 0.5735764363510522656 ) ) ;
#727 = FACE_OUTER_BOUND ( 'NONE', #7562, .T. ) ;
#728 = DIRECTION ( 'NONE',  ( 0.5000000000000022204, 0.8660254037844374864, -0.000000000000000000 ) ) ;
#729 = ORIENTED_EDGE ( 'NONE', *, *, #4099, .T. ) ;
#730 = EDGE_LOOP ( 'NONE', ( #3773, #3925, #4540, #10930 ) ) ;
#731 = DIRECTION ( 'NONE',  ( -0.000000000000000000, 1.000000000000000000, -0.000000000000000000 ) ) ;
#732 = CARTESIAN_POINT ( 'NONE',  ( -4.000000000000000000, -2.512220745329312610, -3.469390707569719901 ) ) ;
#733 = CARTESIAN_POINT ( 'NONE',  ( 23.17052989764754756, 21.62756661655841839, 12.00579112326981246 ) ) ;
#734 = CARTESIAN_POINT ( 'NONE',  ( 4.197393957002303999, 0.8151795401431359833, -3.503767560748935139 ) ) ;
#735 = CARTESIAN_POINT ( 'NONE',  ( -25.98076211353311393, 55.88749999808803182, -7.000000000000072831 ) ) ;
#736 = CARTESIAN_POINT ( 'NONE',  ( -25.98076211353311393, 50.24374999904395622, -3.128098921329806714 ) ) ;
#737 = CARTESIAN_POINT ( 'NONE',  ( 0.1999999999999987899, 0.000000000000000000, 0.000000000000000000 ) ) ;
#738 = DIRECTION ( 'NONE',  ( -0.000000000000000000, -0.000000000000000000, -1.000000000000000000 ) ) ;
#739 = ORIENTED_EDGE ( 'NONE', *, *, #9306, .T. ) ;
#740 = EDGE_CURVE ( 'NONE', #7218, #1417, #8677, .T. ) ;
#741 = CONICAL_SURFACE ( 'NONE', #3236, 4.000000000000000000, 0.8911886515913786111 ) ;
#742 = CARTESIAN_POINT ( 'NONE',  ( 1.767766952966377314, 28.23223304703363112, 14.43750000000000178 ) ) ;
#743 = EDGE_CURVE ( 'NONE', #932, #3081, #7495, .T. ) ;
#744 = DIRECTION ( 'NONE',  ( 0.000000000000000000, -0.5000000000000011102, -0.8660254037844379305 ) ) ;
#745 = CARTESIAN_POINT ( 'NONE',  ( -24.35964822603314772, 54.56041666571061910, -4.064049460664953983 ) ) ;
#746 = CARTESIAN_POINT ( 'NONE',  ( 19.29066956973784386, 17.16581860495888634, 12.00630190750973370 ) ) ;
#747 = CARTESIAN_POINT ( 'NONE',  ( -23.98076211353314235, 52.29999999999986215, -5.000000000000103029 ) ) ;
#748 = ORIENTED_EDGE ( 'NONE', *, *, #5542, .F. ) ;
#749 = EDGE_CURVE ( 'NONE', #8234, #5182, #5392, .T. ) ;
#750 = VERTEX_POINT ( 'NONE', #7844 ) ;
#751 = ORIENTED_EDGE ( 'NONE', *, *, #7672, .T. ) ;
#752 = DIRECTION ( 'NONE',  ( 1.000000000000000000, -0.000000000000000000, -0.000000000000000000 ) ) ;
#753 = EDGE_LOOP ( 'NONE', ( #8453, #4556, #9444, #8263 ) ) ;
#754 = EDGE_CURVE ( 'NONE', #3324, #10078, #215, .T. ) ;
#755 = CARTESIAN_POINT ( 'NONE',  ( 2.982310868301981888, -1.691919446222082568, -3.499999999999999556 ) ) ;
#756 = ORIENTED_EDGE ( 'NONE', *, *, #4402, .T. ) ;
#757 = CARTESIAN_POINT ( 'NONE',  ( 17.65010306112908722, 17.31038946799904465, 12.07741653513508417 ) ) ;
#758 = DIRECTION ( 'NONE',  ( -1.000000000000000000, 0.000000000000000000, 0.000000000000000000 ) ) ;
#759 = PLANE ( 'NONE',  #6344 ) ;
#760 = CARTESIAN_POINT ( 'NONE',  ( 18.97799213218983994, 15.95698123192398477, 12.96557279687576525 ) ) ;
#761 = EDGE_CURVE ( 'NONE', #652, #9304, #1958, .T. ) ;
#762 = AXIS2_PLACEMENT_3D ( 'NONE', #3197, #8099, #3823 ) ;
#763 = LINE ( 'NONE', #4112, #7788 ) ;
#764 = CARTESIAN_POINT ( 'NONE',  ( -27.98076211353308551, 56.00416666475471317, -6.154700538379338504 ) ) ;
#765 = FACE_OUTER_BOUND ( 'NONE', #10921, .T. ) ;
#766 = ORIENTED_EDGE ( 'NONE', *, *, #8949, .T. ) ;
#767 = DIRECTION ( 'NONE',  ( 0.000000000000000000, 1.000000000000000000, 0.000000000000000000 ) ) ;
#768 = ORIENTED_EDGE ( 'NONE', *, *, #5709, .F. ) ;
#769 = CARTESIAN_POINT ( 'NONE',  ( 2.521662442312485819, 32.42808502599335441, 16.99780841526693820 ) ) ;
#770 = ORIENTED_EDGE ( 'NONE', *, *, #8581, .F. ) ;
#771 = ADVANCED_FACE ( 'NONE', ( #9607 ), #4510, .F. ) ;
#772 = EDGE_CURVE ( 'NONE', #647, #318, #5378, .T. ) ;
#773 = CARTESIAN_POINT ( 'NONE',  ( 20.12931512496741249, 22.03068688373604900, 13.00425721518366728 ) ) ;
#774 = CIRCLE ( 'NONE', #5758, 4.499999999999999112 ) ;
#775 = CARTESIAN_POINT ( 'NONE',  ( 22.60611905166032898, 18.24656216730335601, 11.95042449705224819 ) ) ;
#776 = CARTESIAN_POINT ( 'NONE',  ( 29.50000000000000711, -3.999999999999989786, -2.850000000000007194 ) ) ;
#777 = LINE ( 'NONE', #3237, #3403 ) ;
#778 = AXIS2_PLACEMENT_3D ( 'NONE', #10087, #5202, #962 ) ;
#779 = CARTESIAN_POINT ( 'NONE',  ( -2.494791681227495950, 29.73705052183845154, 15.48578750830907147 ) ) ;
#780 = AXIS2_PLACEMENT_3D ( 'NONE', #1700, #10147, #4202 ) ;
#781 = CARTESIAN_POINT ( 'NONE',  ( 3.200000000000000178, 0.000000000000000000, -3.369999999999997886 ) ) ;
#782 = CARTESIAN_POINT ( 'NONE',  ( -27.98076211353308551, 55.30416666475468901, -6.154700538379338504 ) ) ;
#783 = VERTEX_POINT ( 'NONE', #2849 ) ;
#784 = ORIENTED_EDGE ( 'NONE', *, *, #10155, .T. ) ;
#785 = PLANE ( 'NONE',  #286 ) ;
#786 = CIRCLE ( 'NONE', #10023, 2.649999999999992362 ) ;
#787 = DIRECTION ( 'NONE',  ( 0.000000000000000000, 0.000000000000000000, -1.000000000000000000 ) ) ;
#788 = VECTOR ( 'NONE', #2505, 1000.000000000000000 ) ;
#789 = CARTESIAN_POINT ( 'NONE',  ( 21.51635413324704160, 18.70478684647606826, 12.00579112326941988 ) ) ;
#790 = CIRCLE ( 'NONE', #2794, 3.499999999999997780 ) ;
#791 = AXIS2_PLACEMENT_3D ( 'NONE', #5616, #9047, #3159 ) ;
#792 = CARTESIAN_POINT ( 'NONE',  ( -25.44486372867087098, 55.85623925897107256, -7.000000000000071942 ) ) ;
#793 = EDGE_CURVE ( 'NONE', #10021, #7800, #2005, .T. ) ;
#794 = CARTESIAN_POINT ( 'NONE',  ( 0.2500000000000002220, 0.000000000000000000, 0.000000000000000000 ) ) ;
#795 = CARTESIAN_POINT ( 'NONE',  ( -27.60187600103308370, 52.86874999904394912, -5.000000000000103029 ) ) ;
#796 = CARTESIAN_POINT ( 'NONE',  ( 25.71106610644839208, 53.49999999999983658, 14.50000000000000000 ) ) ;
#797 = DIRECTION ( 'NONE',  ( 1.000000000000000000, 0.000000000000000000, 0.000000000000000000 ) ) ;
#798 = VECTOR ( 'NONE', #7045, 1000.000000000000000 ) ;
#799 = ORIENTED_EDGE ( 'NONE', *, *, #6532, .T. ) ;
#800 = CYLINDRICAL_SURFACE ( 'NONE', #6625, 4.000000000000599520 ) ;
#801 = CARTESIAN_POINT ( 'NONE',  ( -27.98076211353308551, 53.26249999808803182, -5.000000000000103029 ) ) ;
#802 = CARTESIAN_POINT ( 'NONE',  ( -25.98076211353310683, 54.96874999904394343, -6.871901078670399343 ) ) ;
#803 = CARTESIAN_POINT ( 'NONE',  ( -5.076455387921338769, 24.47916666666667140, 0.000000000000000000 ) ) ;
#804 = AXIS2_PLACEMENT_3D ( 'NONE', #846, #4248, #10016 ) ;
#805 = B_SPLINE_CURVE_WITH_KNOTS ( 'NONE', 3,
 ( #2324, #1391, #1333, #3057, #5717, #7489 ),
 .UNSPECIFIED., .F., .F.,
 ( 4, 2, 4 ),
 ( 4.336808689942017736E-19, 0.0002095117440854729585, 0.0004190234881709454834 ),
 .UNSPECIFIED. ) ;
#806 = B_SPLINE_CURVE_WITH_KNOTS ( 'NONE', 3,
 ( #4263, #5098, #3194, #3311, #7648, #10148 ),
 .UNSPECIFIED., .F., .F.,
 ( 4, 2, 4 ),
 ( 0.002365888236227995517, 0.003551327329835084114, 0.004736766423442172712 ),
 .UNSPECIFIED. ) ;
#807 = CARTESIAN_POINT ( 'NONE',  ( 19.85760542366876535, 20.31250532737884384, 12.00579112326941988 ) ) ;
#808 = CARTESIAN_POINT ( 'NONE',  ( -27.98076211353308551, 52.70833333333320070, -3.845299461620869330 ) ) ;
#809 = ORIENTED_EDGE ( 'NONE', *, *, #7983, .T. ) ;
#810 = ORIENTED_EDGE ( 'NONE', *, *, #5380, .F. ) ;
#811 = ORIENTED_EDGE ( 'NONE', *, *, #6656, .T. ) ;
#812 = CARTESIAN_POINT ( 'NONE',  ( 29.49999999999999289, 2.000000000000001776, 2.500000000000000000 ) ) ;
#813 = ORIENTED_EDGE ( 'NONE', *, *, #5057, .F. ) ;
#814 = CARTESIAN_POINT ( 'NONE',  ( 29.49999999999999289, 5.000000000000000888, 2.500000000000000000 ) ) ;
#815 = DIRECTION ( 'NONE',  ( 1.000000000000000000, 0.000000000000000000, 0.000000000000000000 ) ) ;
#816 = ORIENTED_EDGE ( 'NONE', *, *, #6670, .T. ) ;
#817 = AXIS2_PLACEMENT_3D ( 'NONE', #4988, #5159, #5980 ) ;
#818 = CARTESIAN_POINT ( 'NONE',  ( 19.66613420429507997, 17.48520406133187066, 11.00732503135576401 ) ) ;
#819 = CARTESIAN_POINT ( 'NONE',  ( -25.98076211353311038, 61.49999999999985789, -1.499999999999510392 ) ) ;
#820 = CARTESIAN_POINT ( 'NONE',  ( -25.71106610644865498, 0.000000000000000000, -9.500000000000000000 ) ) ;
#821 = AXIS2_PLACEMENT_3D ( 'NONE', #8767, #7833, #7722 ) ;
#822 = CARTESIAN_POINT ( 'NONE',  ( -25.98076211353311393, 50.41874999904393917, -3.128098921329806714 ) ) ;
#823 = EDGE_CURVE ( 'NONE', #8525, #1015, #3146, .T. ) ;
#824 = CARTESIAN_POINT ( 'NONE',  ( 15.36174878203077476, 18.17378512388119915, 11.22291988893967840 ) ) ;
#825 = B_SPLINE_CURVE_WITH_KNOTS ( 'NONE', 1,
 ( #3798, #9631 ),
 .UNSPECIFIED., .F., .F.,
 ( 2, 2 ),
 ( 0.000000000000000000, 1.000000000000000000 ),
 .UNSPECIFIED. ) ;
#826 = CYLINDRICAL_SURFACE ( 'NONE', #6009, 7.500000000000000000 ) ;
#827 = CARTESIAN_POINT ( 'NONE',  ( -26.98076211353309972, 55.47916666475470038, -3.267949192431252037 ) ) ;
#828 = DIRECTION ( 'NONE',  ( -1.000000000000000000, 0.000000000000000000, 0.000000000000000000 ) ) ;
#829 = VERTEX_POINT ( 'NONE', #10864 ) ;
#830 = CARTESIAN_POINT ( 'NONE',  ( 6.098637220230963427E-16, -10.00000000000000000, 0.000000000000000000 ) ) ;
#831 = PRODUCT_DEFINITION_SHAPE ( 'NONE', 'NONE',  #11003 ) ;
#832 = ORIENTED_EDGE ( 'NONE', *, *, #10941, .F. ) ;
#833 = CIRCLE ( 'NONE', #5635, 24.99999999999999645 ) ;
#834 = VECTOR ( 'NONE', #10059, 999.9999999999998863 ) ;
#835 = CARTESIAN_POINT ( 'NONE',  ( 1.383578242660657098, 33.52740819067396671, 15.08031658473306891 ) ) ;
#836 = ORIENTED_EDGE ( 'NONE', *, *, #9189, .T. ) ;
#837 = CARTESIAN_POINT ( 'NONE',  ( 19.53332707643461319, 16.11782042516817981, 12.95310296989756260 ) ) ;
#838 = EDGE_CURVE ( 'NONE', #2609, #10326, #4874, .T. ) ;
#839 = EDGE_CURVE ( 'NONE', #8937, #5318, #2844, .T. ) ;
#840 = DIRECTION ( 'NONE',  ( 0.000000000000000000, 0.000000000000000000, -1.000000000000000000 ) ) ;
#841 = AXIS2_PLACEMENT_3D ( 'NONE', #5509, #10615, #4675 ) ;
#842 = COLOUR_RGB ( '', 0.72549020, 0.75294118, 0.79215686) ;
#843 = DIRECTION ( 'NONE',  ( 0.8660254037844374864, -0.5000000000000018874, 0.000000000000000000 ) ) ;
#844 = CARTESIAN_POINT ( 'NONE',  ( -27.60187600103308014, 50.01041666571062194, -5.935950539335252074 ) ) ;
#845 = CARTESIAN_POINT ( 'NONE',  ( 1.035533905932737975, 32.50000000000000711, 13.57812500000000178 ) ) ;
#846 = CARTESIAN_POINT ( 'NONE',  ( 3.200000000000000178, 2.020725942163738686, 3.499999999999999556 ) ) ;
#847 = DIRECTION ( 'NONE',  ( -1.000000000000000000, -6.098637220230963674E-17, 0.000000000000000000 ) ) ;
#848 = CARTESIAN_POINT ( 'NONE',  ( 25.49999999999999645, -3.999999999999986233, -3.349999999999993427 ) ) ;
#849 = ORIENTED_EDGE ( 'NONE', *, *, #4961, .F. ) ;
#850 = ORIENTED_EDGE ( 'NONE', *, *, #2068, .F. ) ;
#851 = AXIS2_PLACEMENT_3D ( 'NONE', #2764, #4948, #10873 ) ;
#852 = CYLINDRICAL_SURFACE ( 'NONE', #1893, 2.149999999999988809 ) ;
#853 = B_SPLINE_CURVE_WITH_KNOTS ( 'NONE', 3,
 ( #2831, #6202, #1987, #5374, #8758, #1473 ),
 .UNSPECIFIED., .F., .F.,
 ( 4, 2, 4 ),
 ( 0.002044882221487568340, 0.003063384235218514964, 0.004081886248949461587 ),
 .UNSPECIFIED. ) ;
#854 = PLANE ( 'NONE',  #9315 ) ;
#855 = STYLED_ITEM ( 'NONE', ( #9750 ), #1910 ) ;
#856 = CARTESIAN_POINT ( 'NONE',  ( 22.69616945897178084, 19.53356342368596898, 12.00579112326941988 ) ) ;
#857 = CARTESIAN_POINT ( 'NONE',  ( -1.035533905932736420, 27.49999999999998934, 15.45312500000000178 ) ) ;
#858 = CARTESIAN_POINT ( 'NONE',  ( 34.90196196521935690, 2.620161469061431880, 3.662783066803843468 ) ) ;
#859 = CARTESIAN_POINT ( 'NONE',  ( -24.35964822603314772, 52.46041666571062478, -4.064049460664953983 ) ) ;
#860 = DIRECTION ( 'NONE',  ( -1.156482317317871478E-16, 1.807003620809174139E-16, 1.000000000000000000 ) ) ;
#861 = CARTESIAN_POINT ( 'NONE',  ( 34.99999999999987210, -9.999999999999998224, -10.50000000000001243 ) ) ;
#862 = DIRECTION ( 'NONE',  ( -1.000000000000000000, 0.000000000000000000, 0.000000000000000000 ) ) ;
#863 = ORIENTED_EDGE ( 'NONE', *, *, #7983, .F. ) ;
#864 = CARTESIAN_POINT ( 'NONE',  ( -4.203833317240879275, -1.627343821129593859, -3.597273115243890818 ) ) ;
#865 = CARTESIAN_POINT ( 'NONE',  ( -30.75045812061784289, 16.50000000000026290, -2.500000000000000000 ) ) ;
#866 = CARTESIAN_POINT ( 'NONE',  ( -24.35964822603314772, 54.73541666571061626, -4.064049460664953983 ) ) ;
#867 = EDGE_CURVE ( 'NONE', #9108, #1634, #6971, .T. ) ;
#868 = CARTESIAN_POINT ( 'NONE',  ( -24.35964822603314772, 55.37708333237728908, -5.935950539335252074 ) ) ;
#869 = CARTESIAN_POINT ( 'NONE',  ( 2.500000000000000000, 1.178949249685218525, 2.041999999999999371 ) ) ;
#870 = CARTESIAN_POINT ( 'NONE',  ( -27.98076211353308551, 51.24999999999986500, -5.000000000000103029 ) ) ;
#871 = ORIENTED_EDGE ( 'NONE', *, *, #9335, .F. ) ;
#872 = ORIENTED_EDGE ( 'NONE', *, *, #9755, .T. ) ;
#873 = DIRECTION ( 'NONE',  ( -0.000000000000000000, 1.000000000000000000, 0.000000000000000000 ) ) ;
#874 = VERTEX_POINT ( 'NONE', #8674 ) ;
#875 = CARTESIAN_POINT ( 'NONE',  ( 2.000000000000000000, 0.000000000000000000, 1.535500000000000087 ) ) ;
#876 = PRESENTATION_STYLE_ASSIGNMENT (( #5720 ) ) ;
#877 = EDGE_LOOP ( 'NONE', ( #6365, #5510 ) ) ;
#878 = DIRECTION ( 'NONE',  ( 1.000000000000000000, 0.000000000000000000, 0.000000000000000000 ) ) ;
#879 = CARTESIAN_POINT ( 'NONE',  ( 29.49999999999999645, -7.999999999999996447, -12.49999999999999822 ) ) ;
#880 = CARTESIAN_POINT ( 'NONE',  ( -25.98076211353311393, 52.03749999808803750, -3.000000000000132339 ) ) ;
#881 = CARTESIAN_POINT ( 'NONE',  ( -24.35964822603314417, 49.89374999904394770, -5.000000000000103029 ) ) ;
#882 = CARTESIAN_POINT ( 'NONE',  ( 22.05490153526506703, 17.93057544254518376, 10.95195840513859231 ) ) ;
#883 = CARTESIAN_POINT ( 'NONE',  ( -3.456897879362374582, 29.45240795142739998, 16.49922112211940117 ) ) ;
#884 = CARTESIAN_POINT ( 'NONE',  ( 25.49999999999999645, -3.999999999999983569, 10.00000000000000888 ) ) ;
#885 = CARTESIAN_POINT ( 'NONE',  ( -27.98076211353308551, 55.42083333142137036, -3.845299461620869330 ) ) ;
#886 = DIRECTION ( 'NONE',  ( 0.000000000000000000, 1.224646799147355672E-16, 1.000000000000000000 ) ) ;
#887 = ORIENTED_EDGE ( 'NONE', *, *, #8923, .F. ) ;
#888 = CARTESIAN_POINT ( 'NONE',  ( -24.98076211353203746, 58.13304142775955086, -3.267949192431878203 ) ) ;
#889 = ORIENTED_EDGE ( 'NONE', *, *, #4930, .T. ) ;
#890 = CARTESIAN_POINT ( 'NONE',  ( -3.500000000000003553, 31.44974746830583356, 16.39062500000000355 ) ) ;
#891 = ORIENTED_EDGE ( 'NONE', *, *, #7285, .T. ) ;
#892 = EDGE_CURVE ( 'NONE', #7431, #6444, #4678, .T. ) ;
#893 = CARTESIAN_POINT ( 'NONE',  ( 21.85833415550051484, 17.65895283167741425, 12.94889058896590583 ) ) ;
#894 =( NAMED_UNIT ( * ) PLANE_ANGLE_UNIT ( ) SI_UNIT ( $, .RADIAN. ) );
#895 = DIRECTION ( 'NONE',  ( 0.000000000000000000, 0.000000000000000000, 1.000000000000000000 ) ) ;
#896 = CARTESIAN_POINT ( 'NONE',  ( 17.59356678224322934, 17.35619608210146581, 12.08212522340233264 ) ) ;
#897 = CARTESIAN_POINT ( 'NONE',  ( -26.79131905728310059, 52.75208333237728198, -6.403925809002825709 ) ) ;
#898 = CARTESIAN_POINT ( 'NONE',  ( -1.767766952966370209, 28.23223304703362402, 15.37500000000000355 ) ) ;
#899 = PLANE ( 'NONE',  #3125 ) ;
#900 = CARTESIAN_POINT ( 'NONE',  ( 25.98076211353311749, 56.49999999999984368, 7.850000000000009415 ) ) ;
#901 = DIRECTION ( 'NONE',  ( 1.000000000000000000, 0.000000000000000000, 0.000000000000000000 ) ) ;
#902 = ADVANCED_FACE ( 'NONE', ( #7791 ), #8557, .F. ) ;
#903 = ORIENTED_EDGE ( 'NONE', *, *, #7998, .F. ) ;
#904 = ORIENTED_EDGE ( 'NONE', *, *, #6155, .T. ) ;
#905 = EDGE_CURVE ( 'NONE', #7610, #10564, #3067, .T. ) ;
#906 = DIRECTION ( 'NONE',  ( -1.000000000000000000, 0.000000000000000000, 0.000000000000000000 ) ) ;
#907 = FACE_OUTER_BOUND ( 'NONE', #4689, .T. ) ;
#908 = CARTESIAN_POINT ( 'NONE',  ( 34.94281041931228771, 2.000000000000002220, -5.301324476612965242 ) ) ;
#909 = CARTESIAN_POINT ( 'NONE',  ( -2.385244779468109755E-15, 32.50000000000000711, 16.15625000000000355 ) ) ;
#910 = PLANE ( 'NONE',  #3395 ) ;
#911 = CARTESIAN_POINT ( 'NONE',  ( -27.60187600103308370, 54.96874999904395054, -5.000000000000103029 ) ) ;
#912 = DIRECTION ( 'NONE',  ( 0.000000000000000000, 1.000000000000000000, 0.000000000000000000 ) ) ;
#913 = CARTESIAN_POINT ( 'NONE',  ( 2.887392608830347207, 2.020725942163738686, 3.499999999999999556 ) ) ;
#914 = LINE ( 'NONE', #2871, #8975 ) ;
#915 = ADVANCED_FACE ( 'NONE', ( #5337 ), #6104, .F. ) ;
#916 = EDGE_LOOP ( 'NONE', ( #9339, #3984, #219, #3158 ) ) ;
#917 = CARTESIAN_POINT ( 'NONE',  ( 29.50000000000000711, -7.999999999999996447, -12.50000000000000000 ) ) ;
#918 = CARTESIAN_POINT ( 'NONE',  ( 34.99999999999987210, 2.000000000000002220, -10.49999999999999822 ) ) ;
#919 = ADVANCED_FACE ( 'NONE', ( #10227 ), #3228, .T. ) ;
#920 = EDGE_CURVE ( 'NONE', #7348, #750, #2720, .T. ) ;
#921 = CARTESIAN_POINT ( 'NONE',  ( -27.60187600103308725, 52.98541666571060915, -5.935950539335252074 ) ) ;
#922 = DIRECTION ( 'NONE',  ( 0.000000000000000000, 0.4999999999999989453, -0.8660254037844391517 ) ) ;
#923 = PRODUCT_DEFINITION_SHAPE ( 'NONE', 'NONE',  #11008 ) ;
#924 = DIRECTION ( 'NONE',  ( 1.000000000000000000, -0.000000000000000000, -0.000000000000000000 ) ) ;
#925 = CARTESIAN_POINT ( 'NONE',  ( -26.98076211353309972, 50.66666666666652930, -3.267949192431252037 ) ) ;
#926 = VECTOR ( 'NONE', #5218, 1000.000000000000114 ) ;
#927 = VERTEX_POINT ( 'NONE', #110 ) ;
#928 = ORIENTED_EDGE ( 'NONE', *, *, #4667, .T. ) ;
#929 = DIRECTION ( 'NONE',  ( -0.000000000000000000, 0.000000000000000000, -1.000000000000000000 ) ) ;
#930 = CARTESIAN_POINT ( 'NONE',  ( 11.99999999999999645, 0.000000000000000000, 1.610000000000000098 ) ) ;
#931 = SHAPE_DEFINITION_REPRESENTATION ( #7149, #75 ) ;
#932 = VERTEX_POINT ( 'NONE', #6897 ) ;
#933 = B_SPLINE_CURVE_WITH_KNOTS ( 'NONE', 3,
 ( #5260, #6137, #1814, #4375, #6864, #9529 ),
 .UNSPECIFIED., .F., .F.,
 ( 4, 2, 4 ),
 ( -3.640115492407174633E-06, 0.0002066546034006553863, 0.0004169493222937179812 ),
 .UNSPECIFIED. ) ;
#934 = FACE_OUTER_BOUND ( 'NONE', #7050, .T. ) ;
#935 = DIRECTION ( 'NONE',  ( -0.000000000000000000, -0.000000000000000000, -1.000000000000000000 ) ) ;
#936 = CARTESIAN_POINT ( 'NONE',  ( -5.560781378645573980, 0.000000000000000000, -4.000000000000000000 ) ) ;
#937 = DIRECTION ( 'NONE',  ( -0.1561119869139967753, 0.9855205127846311530, -0.06616922564517428718 ) ) ;
#938 = ADVANCED_FACE ( 'NONE', ( #10453 ), #10282, .T. ) ;
#939 = CARTESIAN_POINT ( 'NONE',  ( 24.09141472773967507, 22.06251279622207306, 11.95042449705264076 ) ) ;
#940 = CARTESIAN_POINT ( 'NONE',  ( 11.99999999999999645, 0.000000000000000000, 0.000000000000000000 ) ) ;
#941 = CARTESIAN_POINT ( 'NONE',  ( -26.98076211353309972, 55.24583333142137320, -6.732050807568954909 ) ) ;
#942 = DIRECTION ( 'NONE',  ( 0.000000000000000000, 0.000000000000000000, 1.000000000000000000 ) ) ;
#943 = ORIENTED_EDGE ( 'NONE', *, *, #703, .F. ) ;
#944 = CARTESIAN_POINT ( 'NONE',  ( -25.10950799871860184, 58.50805689774887952, -3.198836335995408398 ) ) ;
#945 = ORIENTED_EDGE ( 'NONE', *, *, #2787, .F. ) ;
#946 = CARTESIAN_POINT ( 'NONE',  ( 0.06616922564517879746, 26.50000000000000000, 13.28344158473306713 ) ) ;
#947 = VERTEX_POINT ( 'NONE', #7894 ) ;
#948 = CARTESIAN_POINT ( 'NONE',  ( 21.34179237787287065, 23.66094220255952152, 11.95042449705224819 ) ) ;
#949 = SHAPE_REPRESENTATION_RELATIONSHIP ( 'NONE' , 'NONE' ,  #10603, #6795 ) ;
#950 = CARTESIAN_POINT ( 'NONE',  ( 18.94130700685887447, 16.00034706198404066, 11.96718634320919250 ) ) ;
#951 = CARTESIAN_POINT ( 'NONE',  ( 15.88045857259785087, 19.06928889570832197, 12.24278471274156388 ) ) ;
#952 = CARTESIAN_POINT ( 'NONE',  ( -24.35964822603314772, 50.47708333237728340, -5.935950539335252074 ) ) ;
#953 = EDGE_CURVE ( 'NONE', #1015, #6697, #6053, .T. ) ;
#954 = DIRECTION ( 'NONE',  ( 0.000000000000000000, 1.000000000000000000, 0.000000000000000000 ) ) ;
#955 = CARTESIAN_POINT ( 'NONE',  ( -1.219727444046192735E-16, 2.000000000000000000, -10.49999999999999822 ) ) ;
#956 = DIRECTION ( 'NONE',  ( 0.000000000000000000, 0.000000000000000000, -1.000000000000000000 ) ) ;
#957 = ORIENTED_EDGE ( 'NONE', *, *, #2762, .T. ) ;
#958 = EDGE_LOOP ( 'NONE', ( #2750, #5131, #9096, #1734 ) ) ;
#959 = AXIS2_PLACEMENT_3D ( 'NONE', #6647, #5113, #988 ) ;
#960 = CARTESIAN_POINT ( 'NONE',  ( 18.10462311893278553, 17.05669763433401087, 12.04589798090090902 ) ) ;
#961 = DIRECTION ( 'NONE',  ( -1.000000000000000000, 0.000000000000000000, 0.000000000000000000 ) ) ;
#962 = DIRECTION ( 'NONE',  ( 0.000000000000000000, 0.000000000000000000, -1.000000000000000000 ) ) ;
#963 = CONICAL_SURFACE ( 'NONE', #7532, 4.000000000000000000, 0.8911886515913786111 ) ;
#964 = CARTESIAN_POINT ( 'NONE',  ( -26.98076211353309972, 52.53333333333319644, -6.732050807568954909 ) ) ;
#965 = FACE_OUTER_BOUND ( 'NONE', #258, .T. ) ;
#966 = CARTESIAN_POINT ( 'NONE',  ( -26.79131905728310059, 54.15208333237728056, -6.403925809002825709 ) ) ;
#967 = AXIS2_PLACEMENT_3D ( 'NONE', #10328, #5168, #10996 ) ;
#968 = CARTESIAN_POINT ( 'NONE',  ( 2.550604951803072673, 0.000000000000000000, 0.000000000000000000 ) ) ;
#969 = DIRECTION ( 'NONE',  ( -1.156482317317871478E-16, 0.000000000000000000, 1.000000000000000000 ) ) ;
#970 = DIRECTION ( 'NONE',  ( 0.000000000000000000, 1.000000000000000000, 0.000000000000000000 ) ) ;
#971 = EDGE_LOOP ( 'NONE', ( #10177, #7485, #4128, #4625 ) ) ;
#972 = FILL_AREA_STYLE ('',( #1601 ) ) ;
#973 = AXIS2_PLACEMENT_3D ( 'NONE', #3761, #312, #4606 ) ;
#974 = CARTESIAN_POINT ( 'NONE',  ( -1.101703131577911776, 27.52740819067395250, 16.45093341526693820 ) ) ;
#975 = VECTOR ( 'NONE', #847, 1000.000000000000000 ) ;
#976 = CARTESIAN_POINT ( 'NONE',  ( -3.333333333333335258, 2.694301256218251783, -3.300726591567079815 ) ) ;
#977 = AXIS2_PLACEMENT_3D ( 'NONE', #103, #1834, #2727 ) ;
#978 = CARTESIAN_POINT ( 'NONE',  ( -24.35964822603314772, 55.43541666571061199, -4.064049460664953983 ) ) ;
#979 = ADVANCED_FACE ( 'NONE', ( #1837 ), #5230, .T. ) ;
#980 = CARTESIAN_POINT ( 'NONE',  ( -23.98076211353314235, 50.95833333333318649, -6.154700538379337615 ) ) ;
#981 = EDGE_CURVE ( 'NONE', #3105, #4377, #2174, .T. ) ;
#982 = VECTOR ( 'NONE', #2400, 1000.000000000000000 ) ;
#983 = CARTESIAN_POINT ( 'NONE',  ( 34.99999999999987210, 2.000000000000002220, 15.49999999999999645 ) ) ;
#984 = FACE_OUTER_BOUND ( 'NONE', #2842, .T. ) ;
#985 = CIRCLE ( 'NONE', #10037, 4.000000000000000000 ) ;
#986 = ORIENTED_EDGE ( 'NONE', *, *, #3897, .F. ) ;
#987 = ORIENTED_EDGE ( 'NONE', *, *, #1068, .F. ) ;
#988 = DIRECTION ( 'NONE',  ( 0.000000000000000000, 1.000000000000000000, 0.000000000000000000 ) ) ;
#989 = CARTESIAN_POINT ( 'NONE',  ( 4.200000000000001954, 2.449293598294707893E-16, -2.000000000000000888 ) ) ;
#990 = VERTEX_POINT ( 'NONE', #3562 ) ;
#991 = CARTESIAN_POINT ( 'NONE',  ( 3.061158938895386150, 3.710337782248038341, -0.5735064479040072882 ) ) ;
#992 = AXIS2_PLACEMENT_3D ( 'NONE', #9238, #4978, #5147 ) ;
#993 = CARTESIAN_POINT ( 'NONE',  ( 24.49999999999999289, -3.999999999999986233, -7.767949192431114369 ) ) ;
#994 = CARTESIAN_POINT ( 'NONE',  ( 17.22114890795359798, 16.40384437412513208, 11.05348780010051435 ) ) ;
#995 = DIRECTION ( 'NONE',  ( 1.000000000000000000, -0.000000000000000000, -0.000000000000000000 ) ) ;
#996 = CARTESIAN_POINT ( 'NONE',  ( -27.60187600103308014, 51.00208333237728198, -4.064049460664955760 ) ) ;
#997 = DIRECTION ( 'NONE',  ( 0.000000000000000000, 0.000000000000000000, -1.000000000000000000 ) ) ;
#998 = VERTEX_POINT ( 'NONE', #2847 ) ;
#999 = CARTESIAN_POINT ( 'NONE',  ( 0.000000000000000000, 0.000000000000000000, -4.974599999999998801 ) ) ;
#1000 = AXIS2_PLACEMENT_3D ( 'NONE', #2081, #3534, #1071 ) ;
#1001 = EDGE_LOOP ( 'NONE', ( #342, #7622, #3380, #7323 ) ) ;
#1002 = CARTESIAN_POINT ( 'NONE',  ( 1.449747468305836673, 26.49999999999999289, 15.60937500000000711 ) ) ;
#1003 = ORIENTED_EDGE ( 'NONE', *, *, #8256, .T. ) ;
#1004 = CARTESIAN_POINT ( 'NONE',  ( 19.79393261808261428, 23.04652112618272852, 11.95042449705224819 ) ) ;
#1005 = ADVANCED_FACE ( 'NONE', ( #10335 ), #4662, .F. ) ;
#1006 = CARTESIAN_POINT ( 'NONE',  ( 24.35722724902042202, 20.98982846826517346, 11.95042449705185739 ) ) ;
#1007 = CARTESIAN_POINT ( 'NONE',  ( 19.35452611835372849, 17.20101589911864437, 12.00579185514580338 ) ) ;
#1008 = CARTESIAN_POINT ( 'NONE',  ( -25.98076211353311393, 51.99374999904394912, -6.871901078670400231 ) ) ;
#1009 = CARTESIAN_POINT ( 'NONE',  ( -2.500000000000004885, 29.80321974748363090, 16.48359592357600434 ) ) ;
#1010 = VECTOR ( 'NONE', #8855, 1000.000000000000000 ) ;
#1011 = CARTESIAN_POINT ( 'NONE',  ( -0.06616922564517661864, 33.50000000000000000, 15.15844158473306535 ) ) ;
#1012 = DIRECTION ( 'NONE',  ( 1.000000000000000000, -2.212882687011047826E-16, 0.000000000000000000 ) ) ;
#1013 = CARTESIAN_POINT ( 'NONE',  ( 3.200000000000000178, 0.000000000000000000, 0.000000000000000000 ) ) ;
#1014 = ORIENTED_EDGE ( 'NONE', *, *, #7639, .T. ) ;
#1015 = VERTEX_POINT ( 'NONE', #6180 ) ;
#1016 = LINE ( 'NONE', #10524, #1355 ) ;
#1017 = DIRECTION ( 'NONE',  ( 1.000000000000000000, -0.000000000000000000, -0.000000000000000000 ) ) ;
#1018 = AXIS2_PLACEMENT_3D ( 'NONE', #830, #6007, #6951 ) ;
#1019 = CIRCLE ( 'NONE', #10430, 2.149999999999992362 ) ;
#1020 =( NAMED_UNIT ( * ) SI_UNIT ( $, .STERADIAN. ) SOLID_ANGLE_UNIT ( ) );
#1021 = CARTESIAN_POINT ( 'NONE',  ( -2.500000000000007550, 31.03553390593274131, 16.39062500000000355 ) ) ;
#1022 = DIRECTION ( 'NONE',  ( -0.4338606044657101757, -7.385312362483753893E-05, -0.9009800055708032662 ) ) ;
#1023 = CARTESIAN_POINT ( 'NONE',  ( -24.35964822603314772, 53.97708333237728340, -5.935950539335252074 ) ) ;
#1024 = LINE ( 'NONE', #7035, #2642 ) ;
#1025 = CARTESIAN_POINT ( 'NONE',  ( 0.000000000000000000, 0.000000000000000000, 0.000000000000000000 ) ) ;
#1026 = DIRECTION ( 'NONE',  ( 0.000000000000000000, 1.000000000000000000, 0.000000000000000000 ) ) ;
#1027 = ORIENTED_EDGE ( 'NONE', *, *, #5671, .F. ) ;
#1028 = AXIS2_PLACEMENT_3D ( 'NONE', #5558, #8939, #7269 ) ;
#1029 = COLOUR_RGB ( '', 0.66274510, 0.83137255, 0.94901961) ;
#1030 = CARTESIAN_POINT ( 'NONE',  ( -2.500000000000005773, 29.99999999999999645, 15.21875000000000355 ) ) ;
#1031 = AXIS2_PLACEMENT_3D ( 'NONE', #968, #6031, #7704 ) ;
#1032 = CARTESIAN_POINT ( 'NONE',  ( 1.767766952966372429, 31.76776695296637598, 14.75000000000000355 ) ) ;
#1033 = CARTESIAN_POINT ( 'NONE',  ( -25.17020516978313083, 55.37708333237728198, -3.596074190997380349 ) ) ;
#1034 = CARTESIAN_POINT ( 'NONE',  ( -24.98076211353313170, 54.98333333333319928, -3.267949192431250705 ) ) ;
#1035 = AXIS2_PLACEMENT_3D ( 'NONE', #10048, #7874, #4440 ) ;
#1036 = AXIS2_PLACEMENT_3D ( 'NONE', #884, #10173, #2562 ) ;
#1037 = DIRECTION ( 'NONE',  ( 2.212882687011047826E-16, 1.000000000000000000, -0.000000000000000000 ) ) ;
#1038 = DIRECTION ( 'NONE',  ( 0.5150380749100551547, 0.000000000000000000, -0.8571673007021116675 ) ) ;
#1039 = ORIENTED_EDGE ( 'NONE', *, *, #1517, .F. ) ;
#1040 = ORIENTED_EDGE ( 'NONE', *, *, #5486, .F. ) ;
#1041 = CARTESIAN_POINT ( 'NONE',  ( -27.98076211353308551, 54.69166666666652787, -6.154700538379338504 ) ) ;
#1042 = EDGE_CURVE ( 'NONE', #5004, #1390, #1912, .T. ) ;
#1043 = CARTESIAN_POINT ( 'NONE',  ( 34.99999999999987210, 1.431146867680865853E-14, -12.50000000000000000 ) ) ;
#1044 = PRODUCT_CONTEXT ( 'NONE', #7789, 'mechanical' ) ;
#1045 = ORIENTED_EDGE ( 'NONE', *, *, #7098, .T. ) ;
#1046 = FACE_OUTER_BOUND ( 'NONE', #9517, .T. ) ;
#1047 = CARTESIAN_POINT ( 'NONE',  ( -25.44486372867087809, 54.25626073911683278, -3.000000000000132339 ) ) ;
#1048 = CARTESIAN_POINT ( 'NONE',  ( 19.86895450806392560, 16.41003605044161162, 10.95195963068177392 ) ) ;
#1049 = CARTESIAN_POINT ( 'NONE',  ( -2.474873734152920335, 32.47487373415291501, 16.31250000000000355 ) ) ;
#1050 = CARTESIAN_POINT ( 'NONE',  ( -24.35964822603314772, 53.33541666571061057, -4.064049460664953983 ) ) ;
#1051 = ADVANCED_FACE ( 'NONE', ( #228 ), #4624, .T. ) ;
#1052 = CARTESIAN_POINT ( 'NONE',  ( 0.000000000000000000, -1.178949249685213863, 2.042000000000002924 ) ) ;
#1053 = ORIENTED_EDGE ( 'NONE', *, *, #9284, .T. ) ;
#1054 = DIRECTION ( 'NONE',  ( -1.000000000000000000, 0.000000000000000000, 0.000000000000000000 ) ) ;
#1055 = ORIENTED_EDGE ( 'NONE', *, *, #8721, .T. ) ;
#1056 = CARTESIAN_POINT ( 'NONE',  ( -2.521662442312484931, 32.42808502599334730, 14.06469158473306358 ) ) ;
#1057 = ORIENTED_EDGE ( 'NONE', *, *, #6360, .T. ) ;
#1058 = CARTESIAN_POINT ( 'NONE',  ( 23.34652552892808330, 18.77429515943753202, 11.95042449705224819 ) ) ;
#1059 = EDGE_CURVE ( 'NONE', #10287, #9304, #1463, .T. ) ;
#1060 = CARTESIAN_POINT ( 'NONE',  ( 23.64018263364375017, 19.06693133664117212, 11.95042449705224819 ) ) ;
#1061 = CARTESIAN_POINT ( 'NONE',  ( 22.45328846257175925, 22.40877220821986171, 12.00579112326941988 ) ) ;
#1062 = CARTESIAN_POINT ( 'NONE',  ( -27.60187600103308014, 51.41041666571062052, -5.935950539335252074 ) ) ;
#1063 = PLANE ( 'NONE',  #7417 ) ;
#1064 = CARTESIAN_POINT ( 'NONE',  ( 29.49999999999999645, -3.999999999999986233, -6.649999999999981704 ) ) ;
#1065 = DIRECTION ( 'NONE',  ( -0.000000000000000000, 0.000000000000000000, 1.000000000000000000 ) ) ;
#1066 = ORIENTED_EDGE ( 'NONE', *, *, #8871, .F. ) ;
#1067 = ORIENTED_EDGE ( 'NONE', *, *, #9101, .F. ) ;
#1068 = EDGE_CURVE ( 'NONE', #8576, #3283, #3437, .T. ) ;
#1069 =( REPRESENTATION_RELATIONSHIP ('NONE','NONE', #7540, #6402 ) REPRESENTATION_RELATIONSHIP_WITH_TRANSFORMATION ( #8831 )SHAPE_REPRESENTATION_RELATIONSHIP( ) );
#1070 = DIRECTION ( 'NONE',  ( -0.5735764363510461594, 1.003171929053524747E-16, -0.8191520442889916875 ) ) ;
#1071 = DIRECTION ( 'NONE',  ( 0.000000000000000000, 0.000000000000000000, -1.000000000000000000 ) ) ;
#1072 = SURFACE_STYLE_FILL_AREA ( #8696 ) ;
#1073 = CARTESIAN_POINT ( 'NONE',  ( -26.98076211353408738, 58.13236904469467703, -3.267949192431818695 ) ) ;
#1074 = CARTESIAN_POINT ( 'NONE',  ( -21.21106610644865498, 13.49999999999941913, -2.500000000000000000 ) ) ;
#1075 = PLANE ( 'NONE',  #2989 ) ;
#1076 = LINE ( 'NONE', #10587, #10450 ) ;
#1077 = CARTESIAN_POINT ( 'NONE',  ( -3.472591809326048384, 31.51591669395100936, 17.38843341526693820 ) ) ;
#1078 = CYLINDRICAL_SURFACE ( 'NONE', #1884, 4.500000000000000000 ) ;
#1079 = ORIENTED_EDGE ( 'NONE', *, *, #1783, .T. ) ;
#1080 = B_SPLINE_CURVE_WITH_KNOTS ( 'NONE', 3,
 ( #5653, #8197, #8249, #1587, #5596, #2311, #6574, #636 ),
 .UNSPECIFIED., .F., .F.,
 ( 4, 2, 2, 4 ),
 ( 0.000000000000000000, 0.002450665683189819262, 0.003675998524784728893, 0.004901331366379639391 ),
 .UNSPECIFIED. ) ;
#1081 = CIRCLE ( 'NONE', #4649, 2.767949192431121919 ) ;
#1082 = CARTESIAN_POINT ( 'NONE',  ( 2.500000000000010214, 28.96446609406726225, 14.51562500000000355 ) ) ;
#1083 = CARTESIAN_POINT ( 'NONE',  ( -3.049318610115482207E-16, 5.000000000000000000, 5.500000000000000000 ) ) ;
#1084 = UNCERTAINTY_MEASURE_WITH_UNIT (LENGTH_MEASURE( 1.000000000000000082E-05 ), #3943, 'distance_accuracy_value', 'NONE');
#1085 = FACE_OUTER_BOUND ( 'NONE', #3210, .T. ) ;
#1086 = CARTESIAN_POINT ( 'NONE',  ( -25.44486372867087809, 53.75623925897105693, -7.000000000000075495 ) ) ;
#1087 = CONICAL_SURFACE ( 'NONE', #6767, 4.000000000000000000, 0.8911886515913786111 ) ;
#1088 = CARTESIAN_POINT ( 'NONE',  ( -25.98076211353311038, 59.49999999999985789, -0.9999999999995021760 ) ) ;
#1089 = CARTESIAN_POINT ( 'NONE',  ( -24.98076211353313170, 54.28333333333319644, -3.267949192431250705 ) ) ;
#1090 = B_SPLINE_CURVE_WITH_KNOTS ( 'NONE', 3,
 ( #5226, #10277, #8608, #45, #6100, #3503, #2618, #7786 ),
 .UNSPECIFIED., .F., .F.,
 ( 4, 2, 2, 4 ),
 ( 7.780516681398759253E-20, 0.002450665683189819696, 0.003675998524784729327, 0.004901331366379639391 ),
 .UNSPECIFIED. ) ;
#1091 = ORIENTED_EDGE ( 'NONE', *, *, #8045, .T. ) ;
#1092 = EDGE_CURVE ( 'NONE', #1254, #8525, #5107, .T. ) ;
#1093 = VERTEX_POINT ( 'NONE', #34 ) ;
#1094 = CARTESIAN_POINT ( 'NONE',  ( 30.75045812061784289, 53.49999999999983658, 2.500000000000000000 ) ) ;
#1095 = CARTESIAN_POINT ( 'NONE',  ( 2.000000000000000000, -1.329782007511005837, 0.7677500000000023750 ) ) ;
#1096 = PRODUCT_CONTEXT ( 'NONE', #9837, 'mechanical' ) ;
#1097 = EDGE_LOOP ( 'NONE', ( #5766, #2854, #1150 ) ) ;
#1098 = DIRECTION ( 'NONE',  ( 0.000000000000000000, 1.000000000000000000, 0.000000000000000000 ) ) ;
#1099 = CARTESIAN_POINT ( 'NONE',  ( -26.51666049839535688, 51.71876073720500955, -7.000000000000074607 ) ) ;
#1100 = AXIS2_PLACEMENT_3D ( 'NONE', #6812, #5163, #9482 ) ;
#1101 = ADVANCED_FACE ( 'NONE', ( #4326 ), #7142, .F. ) ;
#1102 = CARTESIAN_POINT ( 'NONE',  ( 21.87443830563928415, 19.02131736398618855, 11.00732503135576401 ) ) ;
#1103 = DIRECTION ( 'NONE',  ( 0.000000000000000000, 0.000000000000000000, 1.000000000000000000 ) ) ;
#1104 = ADVANCED_FACE ( 'NONE', ( #153 ), #7714, .F. ) ;
#1105 = CARTESIAN_POINT ( 'NONE',  ( -24.35964822603314772, 52.63541666571061484, -4.064049460664953983 ) ) ;
#1106 = CARTESIAN_POINT ( 'NONE',  ( -25.98076211353311393, 49.49999999999986500, -3.000000000000131894 ) ) ;
#1107 = VERTEX_POINT ( 'NONE', #3319 ) ;
#1108 = DIRECTION ( 'NONE',  ( 6.098637220230963674E-17, -1.000000000000000000, 0.000000000000000000 ) ) ;
#1109 = EDGE_LOOP ( 'NONE', ( #1439, #1605 ) ) ;
#1110 = CARTESIAN_POINT ( 'NONE',  ( -2.500000000000003997, 29.93383077435482065, 12.97094158473306358 ) ) ;
#1111 = VECTOR ( 'NONE', #4090, 1000.000000000000000 ) ;
#1112 = ORIENTED_EDGE ( 'NONE', *, *, #5214, .F. ) ;
#1113 = CARTESIAN_POINT ( 'NONE',  ( 20.26791470906062997, 16.62008925861079334, 11.95042449705224819 ) ) ;
#1114 =( LENGTH_UNIT ( ) NAMED_UNIT ( * ) SI_UNIT ( .MILLI., .METRE. ) );
#1115 = EDGE_CURVE ( 'NONE', #7952, #8322, #1825, .T. ) ;
#1116 = CARTESIAN_POINT ( 'NONE',  ( 19.79393261808261428, 23.04652112618272852, 11.95042449705224819 ) ) ;
#1117 = EDGE_CURVE ( 'NONE', #4463, #7719, #5019, .T. ) ;
#1118 = CARTESIAN_POINT ( 'NONE',  ( 19.05040816462259556, 17.06282649731835122, 12.00984920396035172 ) ) ;
#1119 = CARTESIAN_POINT ( 'NONE',  ( -25.98076211353311393, 53.74374999904394912, -3.128098921329806714 ) ) ;
#1120 = DIRECTION ( 'NONE',  ( 0.000000000000000000, 0.000000000000000000, -1.000000000000000000 ) ) ;
#1121 = CARTESIAN_POINT ( 'NONE',  ( -25.44486372867087454, 50.25623925897107114, -7.000000000000073719 ) ) ;
#1122 = DIRECTION ( 'NONE',  ( 0.000000000000000000, 0.000000000000000000, 1.000000000000000000 ) ) ;
#1123 = ORIENTED_EDGE ( 'NONE', *, *, #4241, .F. ) ;
#1124 = CARTESIAN_POINT ( 'NONE',  ( 17.45361707773674809, 17.49611573659335662, 12.09524845743996657 ) ) ;
#1125 = CARTESIAN_POINT ( 'NONE',  ( 1.567478505476134606E-15, 4.618802153517012066, -3.433295621305382905 ) ) ;
#1126 = CARTESIAN_POINT ( 'NONE',  ( 5.000000000000000888, 0.000000000000000000, 0.000000000000000000 ) ) ;
#1127 = CARTESIAN_POINT ( 'NONE',  ( 2.500000000000000000, 2.357898499370433054, -1.951563910473907981E-15 ) ) ;
#1128 = FACE_OUTER_BOUND ( 'NONE', #115, .T. ) ;
#1129 = CARTESIAN_POINT ( 'NONE',  ( -27.44132332507749439, 55.71836679508493972, -4.296600267573891685 ) ) ;
#1130 = SURFACE_STYLE_FILL_AREA ( #1928 ) ;
#1131 = CARTESIAN_POINT ( 'NONE',  ( -1.734723475976807094E-15, 33.50000000000000000, 16.15625000000000355 ) ) ;
#1132 = CARTESIAN_POINT ( 'NONE',  ( 34.94281041931228771, 2.000000000000002220, 2.500000000000000000 ) ) ;
#1133 = CIRCLE ( 'NONE', #8225, 4.999999999999997335 ) ;
#1134 = ORIENTED_EDGE ( 'NONE', *, *, #5268, .F. ) ;
#1135 = DIRECTION ( 'NONE',  ( 0.000000000000000000, 0.000000000000000000, 1.000000000000000000 ) ) ;
#1136 = CARTESIAN_POINT ( 'NONE',  ( -2.385244779468109755E-15, 32.50000000000000711, 14.90625000000000355 ) ) ;
#1137 = CARTESIAN_POINT ( 'NONE',  ( -3.456897879362374582, 29.45240795142739998, 16.49922112211940117 ) ) ;
#1138 = CARTESIAN_POINT ( 'NONE',  ( 0.1999999999999987899, 0.000000000000000000, 0.000000000000000000 ) ) ;
#1139 = LINE ( 'NONE', #9759, #4350 ) ;
#1140 = CONICAL_SURFACE ( 'NONE', #4151, 2.059999999999998721, 0.9599310885968738161 ) ;
#1141 = CYLINDRICAL_SURFACE ( 'NONE', #973, 2.149999999999988809 ) ;
#1142 = CARTESIAN_POINT ( 'NONE',  ( -26.79131905728310059, 53.86041666571061626, -3.596074190997381237 ) ) ;
#1143 = DIRECTION ( 'NONE',  ( -0.000000000000000000, 1.000000000000000000, -0.000000000000000000 ) ) ;
#1144 = CARTESIAN_POINT ( 'NONE',  ( -27.98076211353308551, 54.74999999999985789, -5.000000000000103029 ) ) ;
#1145 = AXIS2_PLACEMENT_3D ( 'NONE', #6201, #9587, #410 ) ;
#1146 = ORIENTED_EDGE ( 'NONE', *, *, #9929, .F. ) ;
#1147 = AXIS2_PLACEMENT_3D ( 'NONE', #7692, #126, #9234 ) ;
#1148 =( BOUNDED_CURVE ( )  B_SPLINE_CURVE ( 2, ( #2992, #10744, #9970, #3087, #7467, #6517, #1527, #467, #1368 ),
 .UNSPECIFIED., .F., .F. ) 
 B_SPLINE_CURVE_WITH_KNOTS ( ( 3, 2, 2, 2, 3 ),
 ( 0.3055555555555555802, 0.3148148148148148251, 0.3333333333333333148, 0.3518518518518518601, 0.3611111111111111605 ),
 .UNSPECIFIED. ) 
 CURVE ( )  GEOMETRIC_REPRESENTATION_ITEM ( )  RATIONAL_B_SPLINE_CURVE ( ( 0.9330127018922194093, 0.9330127018922195203, 1.000000000000000000, 0.8660254037844387076, 1.000000000000000000, 0.8660254037844387076, 1.000000000000000000, 0.9330127018922189652, 0.9330127018922194093 ) ) 
 REPRESENTATION_ITEM ( '' )  );
#1149 = CIRCLE ( 'NONE', #5763, 2.149999999999988809 ) ;
#1150 = ORIENTED_EDGE ( 'NONE', *, *, #7639, .F. ) ;
#1151 = CARTESIAN_POINT ( 'NONE',  ( 29.17190429162963738, 6.999999999999999112, 2.500000000000000000 ) ) ;
#1152 = DIRECTION ( 'NONE',  ( 0.8191520442889875797, 0.000000000000000000, 0.5735764363510522656 ) ) ;
#1153 = ORIENTED_EDGE ( 'NONE', *, *, #10578, .F. ) ;
#1154 = CARTESIAN_POINT ( 'NONE',  ( 34.99999999999987210, 1.431146867680865853E-14, 17.49999999999999645 ) ) ;
#1155 = AXIS2_PLACEMENT_3D ( 'NONE', #9102, #8072, #452 ) ;
#1156 = DIRECTION ( 'NONE',  ( 0.000000000000000000, -1.000000000000000000, 0.000000000000000000 ) ) ;
#1157 = AXIS2_PLACEMENT_3D ( 'NONE', #10837, #3223, #1349 ) ;
#1158 = VECTOR ( 'NONE', #7928, 1000.000000000000000 ) ;
#1159 = CARTESIAN_POINT ( 'NONE',  ( 24.30080945327229003, 20.98731269034403368, 10.95195840513820151 ) ) ;
#1160 = EDGE_LOOP ( 'NONE', ( #461, #9264, #6541, #1917, #7943, #7067 ) ) ;
#1161 = CARTESIAN_POINT ( 'NONE',  ( -24.35964822603314772, 51.35208333237728340, -5.935950539335252074 ) ) ;
#1162 = AXIS2_PLACEMENT_3D ( 'NONE', #6518, #2357, #3138 ) ;
#1163 = ORIENTED_EDGE ( 'NONE', *, *, #6957, .T. ) ;
#1164 = CARTESIAN_POINT ( 'NONE',  ( 0.3126073911691312213, -2.020725942164384836, 3.499999999999999556 ) ) ;
#1165 = ORIENTED_EDGE ( 'NONE', *, *, #10968, .F. ) ;
#1166 = CARTESIAN_POINT ( 'NONE',  ( 2.472591809326049272, 31.10170313157791711, 14.92406658473306713 ) ) ;
#1167 = VECTOR ( 'NONE', #6619, 1000.000000000000000 ) ;
#1168 = VERTEX_POINT ( 'NONE', #5983 ) ;
#1169 = CARTESIAN_POINT ( 'NONE',  ( 24.41364504476855402, 20.99234424618630257, 12.94889058896551326 ) ) ;
#1170 = APPLICATION_CONTEXT ( 'automotive_design' ) ;
#1171 = CARTESIAN_POINT ( 'NONE',  ( 2.000000000000000000, 0.8865213383406715941, 1.535499999999999199 ) ) ;
#1172 = CARTESIAN_POINT ( 'NONE',  ( 17.41267794807257374, 17.53706952023173216, 13.10128505860060066 ) ) ;
#1174 = CARTESIAN_POINT ( 'NONE',  ( -26.79131905728310059, 55.08541666571061768, -3.596074190997381237 ) ) ;
#1173 = CIRCLE ( 'NONE', #2600, 4.999999999999997335 ) ;
#1175 = SURFACE_SIDE_STYLE ('',( #8791 ) ) ;
#1176 = CARTESIAN_POINT ( 'NONE',  ( -2.171643655288372443, 3.365003104552320767, 2.541098841762897165E-18 ) ) ;
#1177 = LINE ( 'NONE', #3685, #475 ) ;
#1178 = ORIENTED_EDGE ( 'NONE', *, *, #6407, .F. ) ;
#1179 = EDGE_CURVE ( 'NONE', #681, #3312, #8596, .T. ) ;
#1180 = ORIENTED_EDGE ( 'NONE', *, *, #8476, .T. ) ;
#1181 = EDGE_CURVE ( 'NONE', #3014, #7830, #1772, .T. ) ;
#1182 = CARTESIAN_POINT ( 'NONE',  ( 17.20991452582289583, 17.73983294248524700, 12.11810441208646338 ) ) ;
#1183 = CARTESIAN_POINT ( 'NONE',  ( -25.98076211353311393, 49.49999999999986500, -3.000000000000131894 ) ) ;
#1184 = CARTESIAN_POINT ( 'NONE',  ( -24.98076211353313170, 50.08333333333319359, -3.267949192431250705 ) ) ;
#1185 = CARTESIAN_POINT ( 'NONE',  ( 0.2704726383733979667, 2.234980408443919708E-16, -1.650000000000000355 ) ) ;
#1186 = ORIENTED_EDGE ( 'NONE', *, *, #1270, .F. ) ;
#1187 = CARTESIAN_POINT ( 'NONE',  ( 0.1397399040437575513, 1.362955318038573838, 3.499999999999998224 ) ) ;
#1188 = LINE ( 'NONE', #1248, #10504 ) ;
#1189 = FACE_BOUND ( 'NONE', #5424, .T. ) ;
#1190 = CARTESIAN_POINT ( 'NONE',  ( 2.474873734152922111, 27.52512626584708144, 15.68750000000000355 ) ) ;
#1191 = FACE_OUTER_BOUND ( 'NONE', #4449, .T. ) ;
#1192 = ORIENTED_EDGE ( 'NONE', *, *, #2878, .T. ) ;
#1193 = CARTESIAN_POINT ( 'NONE',  ( -2.500000000000000444, 3.061616997868383634E-16, -25.03750572909317285 ) ) ;
#1194 = ADVANCED_FACE ( 'NONE', ( #10156 ), #7826, .T. ) ;
#1195 = CARTESIAN_POINT ( 'NONE',  ( 0.06616922564517249694, 32.50000000000000711, 15.90405841526694175 ) ) ;
#1196 = VECTOR ( 'NONE', #9291, 1000.000000000000000 ) ;
#1197 = CIRCLE ( 'NONE', #1736, 3.500000000000000000 ) ;
#1198 = CARTESIAN_POINT ( 'NONE',  ( -2.500000000000005773, 29.99999999999999645, 15.21875000000000355 ) ) ;
#1199 = DIRECTION ( 'NONE',  ( -1.000000000000000000, -0.000000000000000000, -0.000000000000000000 ) ) ;
#1200 = CARTESIAN_POINT ( 'NONE',  ( -27.60187600103308370, 55.86681146796336606, -4.629981812462977686 ) ) ;
#1201 = CARTESIAN_POINT ( 'NONE',  ( 23.05579831881754416, 20.86490736922957367, 14.50000000000000000 ) ) ;
#1202 = EDGE_CURVE ( 'NONE', #6168, #6073, #6594, .T. ) ;
#1203 = DIRECTION ( 'NONE',  ( 0.000000000000000000, 0.000000000000000000, 1.000000000000000000 ) ) ;
#1204 = CARTESIAN_POINT ( 'NONE',  ( -25.98076211353311393, 52.16874999904393917, -6.871901078670400231 ) ) ;
#1205 =( BOUNDED_SURFACE ( )  B_SPLINE_SURFACE ( 3, 2, ( 
 ( #2534, #689, #8415 ),
 ( #7530, #9195, #4088 ),
 ( #2598, #9976, #7418 ),
 ( #2362, #9247, #4203 ),
 ( #5977, #1477, #5807 ),
 ( #4872, #8250, #9136 ) ),
 .UNSPECIFIED., .F., .F., .F. ) 
 B_SPLINE_SURFACE_WITH_KNOTS ( ( 4, 2, 4 ),
 ( 3, 3 ),
 ( 0.02027065861071770947, 0.02273072267836921331, 0.02519078674602071716 ),
 ( 0.000000000000000000, 1.000000000000000000 ),
 .UNSPECIFIED. ) 
 GEOMETRIC_REPRESENTATION_ITEM ( )  RATIONAL_B_SPLINE_SURFACE ( (
 ( 1.000000000000000000, 0.8047781708337304885, 1.000000000000000000),
 ( 1.000000000000000000, 0.8123765190705307671, 1.000000000000000000),
 ( 1.000000000000000000, 0.8190656277163975707, 1.000000000000000000),
 ( 1.000000000000000000, 0.8192366903512159348, 1.000000000000000000),
 ( 1.000000000000000000, 0.8126138454302893610, 1.000000000000000000),
 ( 1.000000000000000000, 0.8047712246031417660, 1.000000000000000000) ) ) 
 REPRESENTATION_ITEM ( '' )  SURFACE ( )  );
#1206 = CARTESIAN_POINT ( 'NONE',  ( 34.99999999999987210, -9.999999999999998224, 15.49999999999998934 ) ) ;
#1207 = VECTOR ( 'NONE', #9723, 1000.000000000000000 ) ;
#1208 = COLOUR_RGB ( '', 0.66274510, 0.83137255, 0.94901961) ;
#1209 = LINE ( 'NONE', #7937, #5883 ) ;
#1210 = ORIENTED_EDGE ( 'NONE', *, *, #6774, .F. ) ;
#1211 = AXIS2_PLACEMENT_3D ( 'NONE', #5865, #5096, #7646 ) ;
#1212 = ORIENTED_EDGE ( 'NONE', *, *, #2230, .F. ) ;
#1213 = CARTESIAN_POINT ( 'NONE',  ( -23.98076211353314235, 50.87083333142136610, -6.154700538379337615 ) ) ;
#1214 = DIRECTION ( 'NONE',  ( 0.000000000000000000, 0.000000000000000000, -1.000000000000000000 ) ) ;
#1215 = VERTEX_POINT ( 'NONE', #5273 ) ;
#1216 = EDGE_CURVE ( 'NONE', #3863, #7385, #8026, .T. ) ;
#1217 = VECTOR ( 'NONE', #7964, 1000.000000000000114 ) ;
#1218 = CARTESIAN_POINT ( 'NONE',  ( -25.98076211353311393, 52.03749999808803750, -3.000000000000132783 ) ) ;
#1219 = B_SPLINE_CURVE_WITH_KNOTS ( 'NONE', 3,
 ( #6796, #7640, #1523, #8351, #5856, #69 ),
 .UNSPECIFIED., .F., .F.,
 ( 4, 2, 4 ),
 ( 0.002365888236227967761, 0.003551327329835077609, 0.004736766423442186590 ),
 .UNSPECIFIED. ) ;
#1220 = DIRECTION ( 'NONE',  ( 0.000000000000000000, 0.000000000000000000, 1.000000000000000000 ) ) ;
#1221 = AXIS2_PLACEMENT_3D ( 'NONE', #3907, #4755, #9632 ) ;
#1222 = CARTESIAN_POINT ( 'NONE',  ( 22.00433854689477897, 19.11167697002443333, 11.00732503135576401 ) ) ;
#1223 = SHAPE_REPRESENTATION ( 'socket head cap screw_iso_ISO 4762 M4 x 8 - 8N', ( #308 ), #7601 ) ;
#1224 = ORIENTED_EDGE ( 'NONE', *, *, #5136, .F. ) ;
#1225 = CARTESIAN_POINT ( 'NONE',  ( -27.60187600103308014, 53.80208333237727203, -4.064049460664955760 ) ) ;
#1226 = ORIENTED_EDGE ( 'NONE', *, *, #5735, .F. ) ;
#1227 = CARTESIAN_POINT ( 'NONE',  ( 0.02937408083519319271, -0.6808742863896684039, 3.500000000000000000 ) ) ;
#1228 = VERTEX_POINT ( 'NONE', #4446 ) ;
#1229 = CARTESIAN_POINT ( 'NONE',  ( 1.101703131577918438, 27.52740819067395606, 13.36156658473306535 ) ) ;
#1230 = ORIENTED_EDGE ( 'NONE', *, *, #839, .F. ) ;
#1231 = CARTESIAN_POINT ( 'NONE',  ( 18.81733698050991777, 21.09051435711097966, 10.95195840513859231 ) ) ;
#1232 = ADVANCED_BREP_SHAPE_REPRESENTATION ( '', ( #8973, #308 ), #6353 ) ;
#1233 = CARTESIAN_POINT ( 'NONE',  ( 22.98142095123195716, 18.50759888342988546, 11.95042449705211141 ) ) ;
#1234 = CARTESIAN_POINT ( 'NONE',  ( 19.08509339279509831, 17.01892842213374735, 13.00828316275149099 ) ) ;
#1235 = CARTESIAN_POINT ( 'NONE',  ( -25.98076211353311393, 53.39374999904394770, -6.871901078670400231 ) ) ;
#1236 = CARTESIAN_POINT ( 'NONE',  ( -21.21106610644865498, 13.49999999999941913, -2.500000000000000000 ) ) ;
#1237 = CARTESIAN_POINT ( 'NONE',  ( 21.21106610644839208, 53.49999999999983658, 14.50000000000000000 ) ) ;
#1238 = B_SPLINE_CURVE_WITH_KNOTS ( 'NONE', 3,
 ( #9810, #2255, #5649, #4814, #1472, #4083, #4023, #7411, #10804, #9128, #10026, #2415, #5802, #6798, #7585, #5092, #7642, #71, #4980, #6077, #10307, #17, #9361, #4257, #3418, #10253, #789, #10193, #1759, #1694, #8472, #2590, #856, #3536, #2702, #136, #5971, #5913, #10975, #733, #9296, #3364, #6918, #8579, #6743, #1581, #5150, #2475, #4196, #3306, #8354, #10139 ),
 .UNSPECIFIED., .F., .F.,
 ( 4, 2, 2, 2, 2, 2, 2, 2, 2, 2, 2, 2, 2, 2, 2, 2, 2, 2, 2, 2, 2, 2, 2, 2, 2, 4 ),
 ( 0.05059550242215297977, 0.08415034466753114339, 0.1009277657902202252, 0.1177051869129092931, 0.1353321994545625961, 0.1529592119962158714, 0.1882132370795224774, 0.2234672621628290834, 0.2410942747044824142, 0.2587212872461356894, 0.2827395206008344042, 0.3067577539555331190, 0.3547942206649305485, 0.4028306873743279781, 0.4268489207290267484, 0.4508671540837254077, 0.4680275555186089731, 0.4851879569534925385, 0.5195087598232597248, 0.5881503655627940974, 0.6567919713023284700, 0.7254335770418627316, 0.7940751827813969932, 0.8627167885209312548, 0.9313583942604657384, 1.000000000000000000 ),
 .UNSPECIFIED. ) ;
#1239 = CARTESIAN_POINT ( 'NONE',  ( -25.98076211353311393, 59.00000000000083134, -7.000000000000074607 ) ) ;
#1240 = EDGE_CURVE ( 'NONE', #2458, #625, #4211, .T. ) ;
#1241 = ORIENTED_EDGE ( 'NONE', *, *, #6072, .T. ) ;
#1242 = ORIENTED_EDGE ( 'NONE', *, *, #3599, .T. ) ;
#1243 = CARTESIAN_POINT ( 'NONE',  ( 15.92724728075741680, 19.02250018754875072, 13.24059312800850030 ) ) ;
#1244 = CARTESIAN_POINT ( 'NONE',  ( 2.887392608830349428, 4.041451884327400101, -2.289061810243902218E-14 ) ) ;
#1245 = DIRECTION ( 'NONE',  ( 0.000000000000000000, 0.000000000000000000, -1.000000000000000000 ) ) ;
#1246 = CARTESIAN_POINT ( 'NONE',  ( 0.000000000000000000, 0.000000000000000000, 2.500000000000000000 ) ) ;
#1247 = DIRECTION ( 'NONE',  ( 0.000000000000000000, 0.000000000000000000, 1.000000000000000000 ) ) ;
#1248 = CARTESIAN_POINT ( 'NONE',  ( -23.98076211353314235, 49.49999999999986500, -5.000000000000103029 ) ) ;
#1249 = CARTESIAN_POINT ( 'NONE',  ( 0.000000000000000000, -0.8865213383406694847, 1.535500000000001419 ) ) ;
#1250 = EDGE_CURVE ( 'NONE', #6186, #3385, #6758, .T. ) ;
#1251 = CARTESIAN_POINT ( 'NONE',  ( -24.98076211353312814, 49.61666666666653214, -6.732050807568954909 ) ) ;
#1252 = CARTESIAN_POINT ( 'NONE',  ( -2.474873734152920335, 32.47487373415291501, 13.81250000000000355 ) ) ;
#1253 = CARTESIAN_POINT ( 'NONE',  ( 29.50000000000000711, -3.999999999999989786, 9.999999999999998224 ) ) ;
#1254 = VERTEX_POINT ( 'NONE', #983 ) ;
#1255 = FACE_BOUND ( 'NONE', #7518, .T. ) ;
#1256 = ADVANCED_FACE ( 'NONE', ( #2665 ), #8657, .F. ) ;
#1257 = CARTESIAN_POINT ( 'NONE',  ( -1.383578242660661983, 33.52740819067396671, 15.98218341526694175 ) ) ;
#1258 = CARTESIAN_POINT ( 'NONE',  ( 1.515916693951008254, 33.47259180932604750, 15.82593341526694353 ) ) ;
#1259 = CARTESIAN_POINT ( 'NONE',  ( 22.45328846257175925, 22.40877220821986171, 12.00579112326941988 ) ) ;
#1260 = CARTESIAN_POINT ( 'NONE',  ( -26.11400170334226445, 56.99999999999887734, -7.000000000000075495 ) ) ;
#1261 = CARTESIAN_POINT ( 'NONE',  ( -25.98076211353311393, 53.17499999999985505, -7.000000000000072831 ) ) ;
#1262 = EDGE_CURVE ( 'NONE', #6109, #2863, #8240, .T. ) ;
#1263 = CARTESIAN_POINT ( 'NONE',  ( 29.49999999999999645, 2.000000000000001776, -12.49999999999999822 ) ) ;
#1264 = CARTESIAN_POINT ( 'NONE',  ( -27.60187600103308014, 52.40208333237728056, -4.064049460664955760 ) ) ;
#1265 = CARTESIAN_POINT ( 'NONE',  ( 3.200000000000000178, 3.031088913245510774, -1.750000000000042411 ) ) ;
#1266 = CARTESIAN_POINT ( 'NONE',  ( 2.000000000000000000, 0.000000000000000000, 0.000000000000000000 ) ) ;
#1267 = AXIS2_PLACEMENT_3D ( 'NONE', #2514, #2401, #843 ) ;
#1268 = ORIENTED_EDGE ( 'NONE', *, *, #892, .T. ) ;
#1269 = FACE_OUTER_BOUND ( 'NONE', #1160, .T. ) ;
#1270 = EDGE_CURVE ( 'NONE', #5182, #8762, #6040, .T. ) ;
#1271 = EDGE_CURVE ( 'NONE', #6186, #3429, #7100, .T. ) ;
#1272 = EDGE_CURVE ( 'NONE', #10716, #3226, #5436, .T. ) ;
#1273 = ITEM_DEFINED_TRANSFORMATION ( 'NONE', 'NONE', #2431,  #308 ) ;
#1274 = ORIENTED_EDGE ( 'NONE', *, *, #5530, .F. ) ;
#1275 = DIRECTION ( 'NONE',  ( 1.000000000000000000, 6.098637220230963674E-17, 1.156482317317871478E-16 ) ) ;
#1276 = CONICAL_SURFACE ( 'NONE', #4993, 1664.279482350528269, 1.029744258676657198 ) ;
#1277 = CARTESIAN_POINT ( 'NONE',  ( 29.49999999999999645, 2.000000000000001776, -12.49999999999999822 ) ) ;
#1278 = CARTESIAN_POINT ( 'NONE',  ( 19.52895938645546536, 19.09041019265748673, 10.95195840513859586 ) ) ;
#1279 = ORIENTED_EDGE ( 'NONE', *, *, #10345, .F. ) ;
#1280 = LINE ( 'NONE', #3985, #5818 ) ;
#1281 = ORIENTED_EDGE ( 'NONE', *, *, #1179, .T. ) ;
#1282 = DIRECTION ( 'NONE',  ( -1.000000000000000000, -0.000000000000000000, -0.000000000000000000 ) ) ;
#1283 = ORIENTED_EDGE ( 'NONE', *, *, #6189, .T. ) ;
#1284 = CARTESIAN_POINT ( 'NONE',  ( 2.472591809326049272, 31.10170313157791711, 13.67406658473306535 ) ) ;
#1285 = ORIENTED_EDGE ( 'NONE', *, *, #8430, .T. ) ;
#1286 = CARTESIAN_POINT ( 'NONE',  ( 15.12656308325174415, 18.40897082268132934, 11.24497629747462568 ) ) ;
#1287 =( NAMED_UNIT ( * ) PLANE_ANGLE_UNIT ( ) SI_UNIT ( $, .RADIAN. ) );
#1288 = VECTOR ( 'NONE', #2104, 1000.000000000000000 ) ;
#1289 = EDGE_CURVE ( 'NONE', #829, #1417, #3766, .T. ) ;
#1290 = CARTESIAN_POINT ( 'NONE',  ( -4.000000000000000888, -2.309401076758512694, -3.504269196027526512 ) ) ;
#1291 = CARTESIAN_POINT ( 'NONE',  ( 17.50063742165245984, 17.44909550871243198, 13.09303515564029397 ) ) ;
#1292 = CARTESIAN_POINT ( 'NONE',  ( -4.211140560182196957, 2.431303136016537803, -3.745885042887433514 ) ) ;
#1293 = CARTESIAN_POINT ( 'NONE',  ( -2.000000000000006661, 3.464101615137750834, 0.000000000000000000 ) ) ;
#1294 = DIRECTION ( 'NONE',  ( -0.000000000000000000, -0.000000000000000000, 1.000000000000000000 ) ) ;
#1295 = EDGE_LOOP ( 'NONE', ( #8009, #4620, #5332, #9406 ) ) ;
#1296 = ORIENTED_EDGE ( 'NONE', *, *, #9131, .F. ) ;
#1297 = CARTESIAN_POINT ( 'NONE',  ( 20.00651627240589647, 19.97666299463432438, 12.00579112326824216 ) ) ;
#1298 = CYLINDRICAL_SURFACE ( 'NONE', #5272, 2.649999999999991029 ) ;
#1299 = CARTESIAN_POINT ( 'NONE',  ( -4.000000000000000000, 1.941961291383472732, -0.3515519931180205448 ) ) ;
#1300 = CARTESIAN_POINT ( 'NONE',  ( 34.94281041931228771, 2.000000000000002220, 5.500000000000000000 ) ) ;
#1301 = CARTESIAN_POINT ( 'NONE',  ( 29.49999999999999645, 0.5000000000000135447, -4.999999999999991118 ) ) ;
#1302 = CARTESIAN_POINT ( 'NONE',  ( -25.10912755541051666, 57.49274335135479674, -6.800970407759691305 ) ) ;
#1303 =( NAMED_UNIT ( * ) PLANE_ANGLE_UNIT ( ) SI_UNIT ( $, .RADIAN. ) );
#1304 = CARTESIAN_POINT ( 'NONE',  ( -1.383578242660661983, 33.52740819067396671, 17.23218341526694530 ) ) ;
#1305 = CARTESIAN_POINT ( 'NONE',  ( 21.21106610644839208, 56.49999999999984368, 14.50000000000000000 ) ) ;
#1306 = ORIENTED_EDGE ( 'NONE', *, *, #6540, .T. ) ;
#1307 = LINE ( 'NONE', #3915, #5108 ) ;
#1308 = CARTESIAN_POINT ( 'NONE',  ( 0.9693646802875698354, 27.47259180932603684, 16.60718341526694175 ) ) ;
#1309 = CYLINDRICAL_SURFACE ( 'NONE', #5601, 3.000000000000000000 ) ;
#1310 = CARTESIAN_POINT ( 'NONE',  ( -25.98076211353311393, 50.72499999999985931, -3.000000000000132783 ) ) ;
#1311 = CARTESIAN_POINT ( 'NONE',  ( -23.98076211353314235, 53.67083333142137036, -6.154700538379337615 ) ) ;
#1312 = CARTESIAN_POINT ( 'NONE',  ( -25.44486372867087098, 51.45626073911682852, -3.000000000000133227 ) ) ;
#1313 = CARTESIAN_POINT ( 'NONE',  ( -24.35964822603314417, 51.29374999904394627, -5.000000000000103029 ) ) ;
#1314 = VECTOR ( 'NONE', #2944, 1000.000000000000000 ) ;
#1315 = DIRECTION ( 'NONE',  ( 0.000000000000000000, -1.000000000000000000, 0.000000000000000000 ) ) ;
#1316 = CARTESIAN_POINT ( 'NONE',  ( -3.472371940586054251, -2.614027278893156669, -3.320322319202162031 ) ) ;
#1317 = ORIENTED_EDGE ( 'NONE', *, *, #7967, .T. ) ;
#1318 = CARTESIAN_POINT ( 'NONE',  ( 24.30992024302469900, 5.833333333333329485, 2.500000000000000000 ) ) ;
#1319 = CYLINDRICAL_SURFACE ( 'NONE', #7171, 1.650000000000000355 ) ;
#1320 =( REPRESENTATION_RELATIONSHIP ('NONE','NONE', #7540, #75 ) REPRESENTATION_RELATIONSHIP_WITH_TRANSFORMATION ( #6321 )SHAPE_REPRESENTATION_RELATIONSHIP( ) );
#1321 = ADVANCED_FACE ( 'NONE', ( #414 ), #7150, .F. ) ;
#1322 = ITEM_DEFINED_TRANSFORMATION ( 'NONE', 'NONE', #4022,  #308 ) ;
#1323 = ORIENTED_EDGE ( 'NONE', *, *, #3560, .T. ) ;
#1324 = EDGE_CURVE ( 'NONE', #4849, #2261, #6962, .T. ) ;
#1325 = CARTESIAN_POINT ( 'NONE',  ( 34.94281041931228771, 5.000000000000001776, 2.500000000000000000 ) ) ;
#1326 = CARTESIAN_POINT ( 'NONE',  ( -24.35964822603314417, 49.71874999904395054, -5.000000000000103029 ) ) ;
#1327 = VECTOR ( 'NONE', #7145, 1000.000000000000000 ) ;
#1328 = CARTESIAN_POINT ( 'NONE',  ( 23.59820535295391508, 19.10314065948846718, 10.95195840513859231 ) ) ;
#1329 = AXIS2_PLACEMENT_3D ( 'NONE', #7945, #2115, #8886 ) ;
#1330 = EDGE_LOOP ( 'NONE', ( #5656, #4328, #8187, #2492 ) ) ;
#1331 = CARTESIAN_POINT ( 'NONE',  ( -5.076455387921339657, 24.47916666666667140, -2.499999999999998668 ) ) ;
#1332 = ORIENTED_EDGE ( 'NONE', *, *, #10711, .F. ) ;
#1333 = CARTESIAN_POINT ( 'NONE',  ( 4.024499207728657879, -2.323545700935587988, -3.572172305156509964 ) ) ;
#1334 = VERTEX_POINT ( 'NONE', #314 ) ;
#1335 = CARTESIAN_POINT ( 'NONE',  ( -2.500000000000007550, 31.03553390593274486, 15.14062500000000355 ) ) ;
#1336 = AXIS2_PLACEMENT_3D ( 'NONE', #5007, #8382, #758 ) ;
#1337 = ORIENTED_EDGE ( 'NONE', *, *, #10941, .T. ) ;
#1338 = CONICAL_SURFACE ( 'NONE', #2226, 1.535500000000000087, 1.047197551196590748 ) ;
#1339 = CARTESIAN_POINT ( 'NONE',  ( 16.69520167530635746, 18.25454579299907465, 11.16417930307855677 ) ) ;
#1340 = PRESENTATION_STYLE_ASSIGNMENT (( #8848 ) ) ;
#1341 = CIRCLE ( 'NONE', #10414, 2.000000000000000000 ) ;
#1342 = AXIS2_PLACEMENT_3D ( 'NONE', #10221, #4336, #7725 ) ;
#1343 = FACE_OUTER_BOUND ( 'NONE', #2659, .T. ) ;
#1344 = CARTESIAN_POINT ( 'NONE',  ( 17.25670323398246353, 17.69304423432567930, 13.11591282735340336 ) ) ;
#1345 = B_SPLINE_CURVE_WITH_KNOTS ( 'NONE', 3,
 ( #7291, #5011, #1668, #6404, #560, #9801, #9275, #10642 ),
 .UNSPECIFIED., .F., .F.,
 ( 4, 2, 2, 4 ),
 ( 0.005725059856848645212, 0.006314084072593634418, 0.006903108288338624492, 0.008081156719828603771 ),
 .UNSPECIFIED. ) ;
#1346 = AXIS2_PLACEMENT_3D ( 'NONE', #6919, #7587, #74 ) ;
#1347 = CARTESIAN_POINT ( 'NONE',  ( -25.98076211353311393, 50.98749999808803324, -7.309401076758571314 ) ) ;
#1348 = CIRCLE ( 'NONE', #7555, 1.535500000000000087 ) ;
#1349 = DIRECTION ( 'NONE',  ( 0.000000000000000000, 0.4999999999999921729, -0.8660254037844431485 ) ) ;
#1350 = CARTESIAN_POINT ( 'NONE',  ( -25.98076211353311393, 52.73749999808803324, -3.000000000000132339 ) ) ;
#1351 = VERTEX_POINT ( 'NONE', #3601 ) ;
#1352 = ORIENTED_EDGE ( 'NONE', *, *, #8934, .F. ) ;
#1353 = CARTESIAN_POINT ( 'NONE',  ( 22.03595509826854126, 19.06622527062933870, 12.00579112326941988 ) ) ;
#1354 = EDGE_CURVE ( 'NONE', #183, #9110, #8369, .T. ) ;
#1355 = VECTOR ( 'NONE', #9627, 1000.000000000000000 ) ;
#1356 = LINE ( 'NONE', #3027, #982 ) ;
#1357 = CARTESIAN_POINT ( 'NONE',  ( -26.51666049839535688, 49.99373926088290432, -3.000000000000134115 ) ) ;
#1358 = CARTESIAN_POINT ( 'NONE',  ( -25.71440107481355142, 57.02734599875091703, -6.985969673875411345 ) ) ;
#1359 = DIRECTION ( 'NONE',  ( 1.000000000000000000, 6.098637220230964906E-17, 0.000000000000000000 ) ) ;
#1360 = CARTESIAN_POINT ( 'NONE',  ( -3.472591809326043499, 28.48408330604899064, 13.04906658473306891 ) ) ;
#1361 = CARTESIAN_POINT ( 'NONE',  ( 23.05579831881754416, 20.86490736922957367, 2.500000000000000444 ) ) ;
#1362 = VERTEX_POINT ( 'NONE', #3710 ) ;
#1363 = CARTESIAN_POINT ( 'NONE',  ( -25.98076211353311038, 60.99999999999985789, -5.000000000000102141 ) ) ;
#1364 = AXIS2_PLACEMENT_3D ( 'NONE', #6237, #133, #6290 ) ;
#1365 = CARTESIAN_POINT ( 'NONE',  ( -1.383578242660661983, 33.52740819067396671, 15.98218341526694175 ) ) ;
#1366 = CARTESIAN_POINT ( 'NONE',  ( -4.000000000000000000, 1.700094919196744270, -3.320312364301766017 ) ) ;
#1367 = COLOUR_RGB ( '', 0.09019608, 0.27058824, 0.51372549) ;
#1368 = CARTESIAN_POINT ( 'NONE',  ( -25.98076211353311393, 52.38749999808802471, -7.000000000000072831 ) ) ;
#1369 = CARTESIAN_POINT ( 'NONE',  ( -1.035533905932742860, 32.50000000000000000, 13.73437500000000888 ) ) ;
#1370 = CARTESIAN_POINT ( 'NONE',  ( -1.257172072275743346, 3.892973519171203378, -3.433252694550776862 ) ) ;
#1371 = CARTESIAN_POINT ( 'NONE',  ( -25.17020516978313083, 53.97708333237728340, -3.596074190997380349 ) ) ;
#1372 = CARTESIAN_POINT ( 'NONE',  ( -26.25045812061784289, 16.50000000000026290, -5.000000000000000000 ) ) ;
#1373 = LINE ( 'NONE', #576, #5611 ) ;
#1374 = ORIENTED_EDGE ( 'NONE', *, *, #8914, .F. ) ;
#1375 = PRODUCT_DEFINITION ( 'UNKNOWN', '', #7225, #8335 ) ;
#1376 = CIRCLE ( 'NONE', #5462, 2.149999999999992362 ) ;
#1377 = DIRECTION ( 'NONE',  ( -0.000000000000000000, -0.000000000000000000, 1.000000000000000000 ) ) ;
#1378 = DIRECTION ( 'NONE',  ( 0.000000000000000000, 0.000000000000000000, 1.000000000000000000 ) ) ;
#1379 = CARTESIAN_POINT ( 'NONE',  ( -25.98076211353311393, 49.49999999999986500, -5.000000000000103029 ) ) ;
#1380 = EDGE_CURVE ( 'NONE', #10134, #4348, #10599, .T. ) ;
#1381 = ORIENTED_EDGE ( 'NONE', *, *, #2352, .F. ) ;
#1382 = CARTESIAN_POINT ( 'NONE',  ( -24.35964822603314772, 52.05208333237727913, -5.935950539335252074 ) ) ;
#1383 = CARTESIAN_POINT ( 'NONE',  ( -27.60187600103308725, 51.41041666571062052, -5.935950539335252074 ) ) ;
#1384 = VECTOR ( 'NONE', #5130, 1000.000000000000000 ) ;
#1385 = CARTESIAN_POINT ( 'NONE',  ( 18.79784185921769790, 16.99560944861731215, 12.01584860934582366 ) ) ;
#1386 = VERTEX_POINT ( 'NONE', #2997 ) ;
#1387 = B_SPLINE_CURVE_WITH_KNOTS ( 'NONE', 3,
 ( #1672, #888, #4236, #944, #3458, #6839, #8452, #7735, #114, #2629 ),
 .UNSPECIFIED., .F., .F.,
 ( 4, 2, 2, 2, 4 ),
 ( 0.001591453205566317926, 0.001988835618581903577, 0.002386218031597489228, 0.002783600444613075313, 0.003180982857628660964 ),
 .UNSPECIFIED. ) ;
#1388 = EDGE_CURVE ( 'NONE', #8904, #8565, #9707, .T. ) ;
#1389 = CARTESIAN_POINT ( 'NONE',  ( 34.94281041931228771, 2.000000000000002220, 5.500000000000000000 ) ) ;
#1390 = VERTEX_POINT ( 'NONE', #1088 ) ;
#1391 = CARTESIAN_POINT ( 'NONE',  ( 4.000000000000003553, -2.309401076758513138, -3.504271511726786859 ) ) ;
#1392 = ORIENTED_EDGE ( 'NONE', *, *, #1408, .F. ) ;
#1393 = EDGE_CURVE ( 'NONE', #9720, #9782, #10519, .T. ) ;
#1394 = CIRCLE ( 'NONE', #1028, 0.2000000000000000944 ) ;
#1395 = DIRECTION ( 'NONE',  ( 0.000000000000000000, 0.000000000000000000, 1.000000000000000000 ) ) ;
#1396 =( NAMED_UNIT ( * ) PLANE_ANGLE_UNIT ( ) SI_UNIT ( $, .RADIAN. ) );
#1397 = ORIENTED_EDGE ( 'NONE', *, *, #4683, .T. ) ;
#1398 = VECTOR ( 'NONE', #912, 1000.000000000000000 ) ;
#1399 = CARTESIAN_POINT ( 'NONE',  ( 19.42818427286271898, 22.60367925258928068, 10.95195840513898489 ) ) ;
#1400 = FACE_OUTER_BOUND ( 'NONE', #10325, .T. ) ;
#1401 = CARTESIAN_POINT ( 'NONE',  ( 23.09245737654782360, 19.89859478643763069, 13.00425721518307753 ) ) ;
#1402 = EDGE_CURVE ( 'NONE', #6697, #1254, #6987, .T. ) ;
#1403 = CARTESIAN_POINT ( 'NONE',  ( -27.98076211353308551, 53.26249999808803182, -5.000000000000103029 ) ) ;
#1404 = CARTESIAN_POINT ( 'NONE',  ( 34.94281041931228771, 2.000000000000002665, -5.301324476612966130 ) ) ;
#1405 = CARTESIAN_POINT ( 'NONE',  ( 2.000000000000000000, 1.773042676681340524, -2.059984127722458425E-15 ) ) ;
#1406 = VERTEX_POINT ( 'NONE', #4609 ) ;
#1407 = ORIENTED_EDGE ( 'NONE', *, *, #120, .T. ) ;
#1408 = EDGE_CURVE ( 'NONE', #10875, #10068, #10636, .T. ) ;
#1409 = CARTESIAN_POINT ( 'NONE',  ( 19.16668011427331919, 17.04844365417888596, 13.00677669558776550 ) ) ;
#1410 = PLANE ( 'NONE',  #7732 ) ;
#1411 = CARTESIAN_POINT ( 'NONE',  ( -27.78269984933782411, 56.11211482050296695, -4.132232521764788835 ) ) ;
#1412 = CARTESIAN_POINT ( 'NONE',  ( 3.200000000000000178, 3.031088913245510774, -1.750000000000042411 ) ) ;
#1413 = CARTESIAN_POINT ( 'NONE',  ( 21.21106610644839208, 56.49999999999984368, 2.500000000000000000 ) ) ;
#1414 = CARTESIAN_POINT ( 'NONE',  ( -3.446545381698513655, 29.38705359262400663, 15.50141270685246830 ) ) ;
#1415 = DIRECTION ( 'NONE',  ( -0.000000000000000000, 0.000000000000000000, 1.000000000000000000 ) ) ;
#1416 = ADVANCED_FACE ( 'NONE', ( #2154 ), #1999, .F. ) ;
#1417 = VERTEX_POINT ( 'NONE', #5545 ) ;
#1418 = DIRECTION ( 'NONE',  ( 0.000000000000000000, 0.000000000000000000, 1.000000000000000000 ) ) ;
#1419 = VERTEX_POINT ( 'NONE', #8880 ) ;
#1420 = CARTESIAN_POINT ( 'NONE',  ( -2.527408190673963162, 29.03063531971243094, 16.29468341526694530 ) ) ;
#1421 = DIRECTION ( 'NONE',  ( 1.000000000000000000, 0.000000000000000000, 0.000000000000000000 ) ) ;
#1422 = CARTESIAN_POINT ( 'NONE',  ( -23.98076211353314235, 49.49999999999986500, -5.000000000000103029 ) ) ;
#1423 = CARTESIAN_POINT ( 'NONE',  ( 4.197393957002303999, 7.772902908466098641E-14, -3.503767560748929810 ) ) ;
#1424 = CARTESIAN_POINT ( 'NONE',  ( -1.360585162435467455, 4.061296242128285883, -3.505054077164959203 ) ) ;
#1425 = CARTESIAN_POINT ( 'NONE',  ( -26.79131905728310059, 51.58541666571061768, -3.596074190997381237 ) ) ;
#1426 = CARTESIAN_POINT ( 'NONE',  ( 3.200000000000000178, -0.3416191432521806237, 3.499999999999999112 ) ) ;
#1427 = CARTESIAN_POINT ( 'NONE',  ( 0.1410422978106145031, -4.700232962125109104, -3.687027686973628704 ) ) ;
#1428 = EDGE_LOOP ( 'NONE', ( #3496, #8625, #535, #6616 ) ) ;
#1429 = CARTESIAN_POINT ( 'NONE',  ( -3.500000000000003109, 29.99999999999999645, 13.96875000000000355 ) ) ;
#1430 = CYLINDRICAL_SURFACE ( 'NONE', #2561, 1.999999999999971356 ) ;
#1431 = DIRECTION ( 'NONE',  ( -0.000000000000000000, -0.000000000000000000, 1.000000000000000000 ) ) ;
#1432 = CARTESIAN_POINT ( 'NONE',  ( -26.79131905728310059, 55.08541666571061768, -3.596074190997381237 ) ) ;
#1433 = EDGE_CURVE ( 'NONE', #7860, #7488, #1942, .T. ) ;
#1434 = CARTESIAN_POINT ( 'NONE',  ( 16.11564427137601285, 18.83410319690818824, 12.22072830420661660 ) ) ;
#1435 = CARTESIAN_POINT ( 'NONE',  ( -27.60187600103308014, 54.32708333237728482, -4.064049460664955760 ) ) ;
#1436 = UNCERTAINTY_MEASURE_WITH_UNIT (LENGTH_MEASURE( 1.000000000000000082E-05 ), #6013, 'distance_accuracy_value', 'NONE');
#1437 = VERTEX_POINT ( 'NONE', #7881 ) ;
#1438 = DIRECTION ( 'NONE',  ( -0.000000000000000000, -0.000000000000000000, -1.000000000000000000 ) ) ;
#1439 = ORIENTED_EDGE ( 'NONE', *, *, #8318, .F. ) ;
#1440 = DIRECTION ( 'NONE',  ( 0.000000000000000000, 0.000000000000000000, -1.000000000000000000 ) ) ;
#1441 = ORIENTED_EDGE ( 'NONE', *, *, #5196, .T. ) ;
#1442 = CARTESIAN_POINT ( 'NONE',  ( -2.500000000000007550, 31.03553390593274486, 16.39062500000000355 ) ) ;
#1443 = FILL_AREA_STYLE ('',( #6436 ) ) ;
#1444 = VECTOR ( 'NONE', #10419, 1000.000000000000000 ) ;
#1445 = ORIENTED_EDGE ( 'NONE', *, *, #6596, .F. ) ;
#1446 = CARTESIAN_POINT ( 'NONE',  ( 21.07346791105437589, 22.52558620363005915, 11.00732503135576401 ) ) ;
#1447 = EDGE_CURVE ( 'NONE', #3727, #10063, #9589, .T. ) ;
#1448 = CARTESIAN_POINT ( 'NONE',  ( 3.999999999999999112, 2.309401076758497595, -3.504271511726784194 ) ) ;
#1449 = EDGE_CURVE ( 'NONE', #7957, #3879, #3596, .T. ) ;
#1450 = CARTESIAN_POINT ( 'NONE',  ( 23.83741617020655212, 22.59052263540754524, 12.94889058896590583 ) ) ;
#1451 = CARTESIAN_POINT ( 'NONE',  ( -23.98076211353314235, 51.57083333142137604, -6.154700538379337615 ) ) ;
#1452 = DIRECTION ( 'NONE',  ( -0.000000000000000000, -0.000000000000000000, -1.000000000000000000 ) ) ;
#1453 = DIRECTION ( 'NONE',  ( 1.000000000000000000, -0.000000000000000000, -0.000000000000000000 ) ) ;
#1454 = ORIENTED_EDGE ( 'NONE', *, *, #120, .F. ) ;
#1455 = CARTESIAN_POINT ( 'NONE',  ( 2.428085025993357071, 27.47833755768751374, 15.43530841526694175 ) ) ;
#1456 = VERTEX_POINT ( 'NONE', #1206 ) ;
#1457 = CARTESIAN_POINT ( 'NONE',  ( 20.76856923708738734, 18.11717751085002703, 13.00425721518307576 ) ) ;
#1458 = EDGE_CURVE ( 'NONE', #10907, #3061, #1080, .T. ) ;
#1459 = EDGE_CURVE ( 'NONE', #7662, #1215, #7307, .T. ) ;
#1460 = EDGE_CURVE ( 'NONE', #4949, #8739, #2259, .T. ) ;
#1461 = CARTESIAN_POINT ( 'NONE',  ( -24.98076211353312814, 52.41666666666652930, -6.732050807568954909 ) ) ;
#1462 = CARTESIAN_POINT ( 'NONE',  ( 34.64101615137754919, 5.000000000000002665, 2.500000000000000000 ) ) ;
#1463 = CIRCLE ( 'NONE', #2896, 2.149999999999992362 ) ;
#1464 = CARTESIAN_POINT ( 'NONE',  ( -26.98076211353408382, 57.99999999999985789, -3.267949192431818251 ) ) ;
#1465 = CARTESIAN_POINT ( 'NONE',  ( 2.527408190673965382, 29.03063531971243449, 13.51781658473306713 ) ) ;
#1466 = CARTESIAN_POINT ( 'NONE',  ( -2.059999999999998721, 2.522772406243545965E-16, -0.3080913168122742518 ) ) ;
#1467 = EDGE_LOOP ( 'NONE', ( #9505, #5732, #9792, #6843, #4204, #8776 ) ) ;
#1468 = CARTESIAN_POINT ( 'NONE',  ( -27.98076211353308551, 55.42083333142136325, -3.845299461620869330 ) ) ;
#1469 = ORIENTED_EDGE ( 'NONE', *, *, #9598, .F. ) ;
#1470 = CARTESIAN_POINT ( 'NONE',  ( -0.06616922564517033201, 27.49999999999998934, 16.52905841526693820 ) ) ;
#1471 = LINE ( 'NONE', #10802, #4745 ) ;
#1472 = CARTESIAN_POINT ( 'NONE',  ( 17.20991452582289583, 17.73983294248524700, 12.11810441208646338 ) ) ;
#1473 = CARTESIAN_POINT ( 'NONE',  ( 0.3126073911696294338, 2.020725942163657862, -3.499999999999999556 ) ) ;
#1474 = CARTESIAN_POINT ( 'NONE',  ( 21.55579831881754416, 20.86490736922957367, 14.50000000000000000 ) ) ;
#1475 = CARTESIAN_POINT ( 'NONE',  ( -24.35964822603314417, 51.11874999904394912, -5.000000000000103029 ) ) ;
#1476 = DIRECTION ( 'NONE',  ( 1.000000000000000000, 0.000000000000000000, 0.000000000000000000 ) ) ;
#1477 = CARTESIAN_POINT ( 'NONE',  ( 4.000000000001088907, 1.658577278524410170, -3.531553309554541720 ) ) ;
#1478 = EDGE_LOOP ( 'NONE', ( #5965, #8680, #5001 ) ) ;
#1479 = CARTESIAN_POINT ( 'NONE',  ( -1.449747468305830678, 26.49999999999999289, 15.45312500000000178 ) ) ;
#1480 = CARTESIAN_POINT ( 'NONE',  ( 5.000000000000000888, 4.250000000000000000, 0.000000000000000000 ) ) ;
#1481 = CARTESIAN_POINT ( 'NONE',  ( -27.60187600103308725, 51.00208333237728198, -4.064049460664955760 ) ) ;
#1482 = CARTESIAN_POINT ( 'NONE',  ( -27.60187600103308725, 52.81041666571061199, -5.935950539335252074 ) ) ;
#1483 = CARTESIAN_POINT ( 'NONE',  ( 19.55162244606592381, 17.33808635661342024, 12.00579012602852735 ) ) ;
#1484 = CARTESIAN_POINT ( 'NONE',  ( -27.60187600103308370, 54.26874999904394770, -5.000000000000103029 ) ) ;
#1485 = ORIENTED_EDGE ( 'NONE', *, *, #1289, .F. ) ;
#1486 = CARTESIAN_POINT ( 'NONE',  ( -24.35964822603314772, 55.55208333237727913, -5.935950539335252074 ) ) ;
#1487 = VERTEX_POINT ( 'NONE', #7258 ) ;
#1488 = AXIS2_PLACEMENT_3D ( 'NONE', #9432, #873, #7663 ) ;
#1489 = VERTEX_POINT ( 'NONE', #4933 ) ;
#1490 = FACE_OUTER_BOUND ( 'NONE', #9004, .T. ) ;
#1491 = VERTEX_POINT ( 'NONE', #6470 ) ;
#1492 = DIRECTION ( 'NONE',  ( 0.000000000000000000, 8.326672684688671588E-17, 1.000000000000000000 ) ) ;
#1493 = VERTEX_POINT ( 'NONE', #5806 ) ;
#1494 = CARTESIAN_POINT ( 'NONE',  ( 16.74199038346592872, 18.20775708483950694, 12.16198771834549497 ) ) ;
#1495 =( NAMED_UNIT ( * ) SI_UNIT ( $, .STERADIAN. ) SOLID_ANGLE_UNIT ( ) );
#1496 = VECTOR ( 'NONE', #2306, 1000.000000000000000 ) ;
#1497 = CARTESIAN_POINT ( 'NONE',  ( 0.000000000000000000, 0.000000000000000000, -4.694516984716113228 ) ) ;
#1498 = AXIS2_PLACEMENT_3D ( 'NONE', #4277, #6937, #2614 ) ;
#1499 = CARTESIAN_POINT ( 'NONE',  ( 1.243802165048773611, -3.900692638707475624, -3.223146290109810241 ) ) ;
#1500 = CARTESIAN_POINT ( 'NONE',  ( 23.58716357997163016, 18.92604383881832675, 12.94889058896590583 ) ) ;
#1501 = CARTESIAN_POINT ( 'NONE',  ( -26.98076211353309972, 51.97916666475470038, -3.267949192431252037 ) ) ;
#1502 = AXIS2_PLACEMENT_3D ( 'NONE', #5432, #7146, #10434 ) ;
#1503 = CARTESIAN_POINT ( 'NONE',  ( 34.69578914996070296, 4.608685395970379517, -2.519144107514304398 ) ) ;
#1504 = CARTESIAN_POINT ( 'NONE',  ( -26.98076211353309972, 51.27916666475469754, -3.267949192431252037 ) ) ;
#1505 = ORIENTED_EDGE ( 'NONE', *, *, #5333, .F. ) ;
#1506 = CARTESIAN_POINT ( 'NONE',  ( -0.06616922564517119243, 26.49999999999999289, 15.27905841526694175 ) ) ;
#1507 = VECTOR ( 'NONE', #9328, 1000.000000000000114 ) ;
#1508 = VERTEX_POINT ( 'NONE', #4029 ) ;
#1509 = CARTESIAN_POINT ( 'NONE',  ( 16.23764702455707720, 17.29788688137487185, 13.14516836485838169 ) ) ;
#1510 = VECTOR ( 'NONE', #4752, 1000.000000000000000 ) ;
#1511 = FACE_OUTER_BOUND ( 'NONE', #6548, .T. ) ;
#1512 = CARTESIAN_POINT ( 'NONE',  ( -25.98076211353311393, 49.49999999999986500, -7.000000000000074607 ) ) ;
#1514 = DIRECTION ( 'NONE',  ( 0.000000000000000000, 0.000000000000000000, 1.000000000000000000 ) ) ;
#1513 = AXIS2_PLACEMENT_3D ( 'NONE', #3252, #4934, #862 ) ;
#1515 = CARTESIAN_POINT ( 'NONE',  ( 1.720978244806805169, 31.81455566112594013, 12.50219158473306358 ) ) ;
#1516 = FACE_OUTER_BOUND ( 'NONE', #7546, .T. ) ;
#1517 = EDGE_CURVE ( 'NONE', #233, #4272, #4770, .T. ) ;
#1518 = EDGE_LOOP ( 'NONE', ( #2852, #7234, #3175, #5621, #9061 ) ) ;
#1519 = CARTESIAN_POINT ( 'NONE',  ( 3.199999999999992628, -3.375361811986524074, -1.153701847711610551 ) ) ;
#1520 = ADVANCED_FACE ( 'NONE', ( #575 ), #4820, .F. ) ;
#1521 = VERTEX_POINT ( 'NONE', #7416 ) ;
#1522 = CONICAL_SURFACE ( 'NONE', #2060, 4.624785217660733139, 1.047197551196604071 ) ;
#1523 = CARTESIAN_POINT ( 'NONE',  ( 1.317756351988342622, -3.857995168970215438, -0.04852650426602527628 ) ) ;
#1524 = B_SPLINE_CURVE_WITH_KNOTS ( 'NONE', 3,
 ( #7671, #105, #9772, #10661, #3667, #10449 ),
 .UNSPECIFIED., .F., .F.,
 ( 4, 2, 4 ),
 ( 0.002044882221487540584, 0.003063384235218501086, 0.004081886248949461587 ),
 .UNSPECIFIED. ) ;
#1525 = AXIS2_PLACEMENT_3D ( 'NONE', #8463, #2517, #9914 ) ;
#1526 = DIRECTION ( 'NONE',  ( 1.000000000000000000, 0.000000000000000000, 0.000000000000000000 ) ) ;
#1527 = CARTESIAN_POINT ( 'NONE',  ( -24.98076211353312814, 52.32916666475470180, -6.732050807568954909 ) ) ;
#1528 = DIRECTION ( 'NONE',  ( 4.312387734421982522E-17, -0.7071067811865462405, 0.7071067811865489050 ) ) ;
#1529 = FACE_OUTER_BOUND ( 'NONE', #4996, .T. ) ;
#1530 = CARTESIAN_POINT ( 'NONE',  ( -27.60187600103308014, 50.82708333237729192, -4.064049460664955760 ) ) ;
#1531 = DIRECTION ( 'NONE',  ( -1.000000000000000000, -0.000000000000000000, -0.000000000000000000 ) ) ;
#1532 = CARTESIAN_POINT ( 'NONE',  ( 5.621179405865835754, 34.96511249490581008, 2.500000000000000000 ) ) ;
#1533 = EDGE_CURVE ( 'NONE', #2047, #9268, #472, .T. ) ;
#1534 = ORIENTED_EDGE ( 'NONE', *, *, #4741, .F. ) ;
#1535 = CARTESIAN_POINT ( 'NONE',  ( 3.903127820947815962E-15, 26.49999999999999289, 15.53125000000000355 ) ) ;
#1536 = CARTESIAN_POINT ( 'NONE',  ( 2.500000000000000000, 1.178949249685213863, -2.042000000000001148 ) ) ;
#1537 = EDGE_CURVE ( 'NONE', #9017, #10440, #7362, .T. ) ;
#1538 = CARTESIAN_POINT ( 'NONE',  ( -25.17020516978313083, 51.17708333237727913, -3.596074190997380349 ) ) ;
#1539 = CARTESIAN_POINT ( 'NONE',  ( -24.35964822603314772, 51.87708333237728198, -5.935950539335252074 ) ) ;
#1540 = CARTESIAN_POINT ( 'NONE',  ( 17.20991452582289583, 17.73983294248524700, 12.11810441208646338 ) ) ;
#1541 = VECTOR ( 'NONE', #2747, 1000.000000000000000 ) ;
#1542 = AXIS2_PLACEMENT_3D ( 'NONE', #9267, #6822, #654 ) ;
#1543 = CARTESIAN_POINT ( 'NONE',  ( -24.98076211353313170, 52.18333333333320212, -3.267949192431250705 ) ) ;
#1544 = ORIENTED_EDGE ( 'NONE', *, *, #1599, .F. ) ;
#1545 = ORIENTED_EDGE ( 'NONE', *, *, #7499, .T. ) ;
#1547 = EDGE_LOOP ( 'NONE', ( #5224, #6437, #4786, #1754 ) ) ;
#1546 = EDGE_CURVE ( 'NONE', #998, #4861, #8541, .T. ) ;
#1548 = ORIENTED_EDGE ( 'NONE', *, *, #6325, .T. ) ;
#1549 = CARTESIAN_POINT ( 'NONE',  ( -30.31088913245546124, 17.49999999999980815, 2.500000000000000000 ) ) ;
#1550 = CARTESIAN_POINT ( 'NONE',  ( 39.00000000000004263, -4.000000000000047073, -4.999999999999680256 ) ) ;
#1551 = ORIENTED_EDGE ( 'NONE', *, *, #2352, .T. ) ;
#1553 = CARTESIAN_POINT ( 'NONE',  ( 22.41005638895160601, 19.39388128063383476, 11.00732503135576401 ) ) ;
#1552 = CIRCLE ( 'NONE', #7059, 2.149999999999990585 ) ;
#1554 = AXIS2_PLACEMENT_3D ( 'NONE', #2026, #4533, #9634 ) ;
#1555 = CARTESIAN_POINT ( 'NONE',  ( 29.49999999999999645, -3.999999999999986233, -3.350000000000001421 ) ) ;
#1556 = CARTESIAN_POINT ( 'NONE',  ( 3.199999999999999734, -3.031088913245509886, 1.750000000000043077 ) ) ;
#1557 = CARTESIAN_POINT ( 'NONE',  ( 24.37916169550391032, 20.40431285142311424, 12.94889058896590761 ) ) ;
#1558 = CARTESIAN_POINT ( 'NONE',  ( -24.98076211353313170, 51.39583333142136468, -3.267949192431250705 ) ) ;
#1559 = CIRCLE ( 'NONE', #7784, 2.041999999999999815 ) ;
#1560 = CARTESIAN_POINT ( 'NONE',  ( 25.58039891549807976, 2.000000000000001776, 2.500000000000000000 ) ) ;
#1561 = CARTESIAN_POINT ( 'NONE',  ( -4.211140560182196957, 2.431303136016537803, -3.745885042887433514 ) ) ;
#1562 = UNCERTAINTY_MEASURE_WITH_UNIT (LENGTH_MEASURE( 1.000000000000000082E-05 ), #2671, 'distance_accuracy_value', 'NONE');
#1563 = ORIENTED_EDGE ( 'NONE', *, *, #6544, .T. ) ;
#1564 = AXIS2_PLACEMENT_3D ( 'NONE', #8387, #2187, #5889 ) ;
#1565 = CARTESIAN_POINT ( 'NONE',  ( -0.06616922564517119243, 26.49999999999999289, 16.52905841526693820 ) ) ;
#1566 = VERTEX_POINT ( 'NONE', #3922 ) ;
#1567 = CARTESIAN_POINT ( 'NONE',  ( 23.18216631463591781, 20.05868775325893338, 13.00425721518307753 ) ) ;
#1568 = VECTOR ( 'NONE', #954, 1000.000000000000000 ) ;
#1569 = FACE_OUTER_BOUND ( 'NONE', #3007, .T. ) ;
#1570 = CARTESIAN_POINT ( 'NONE',  ( 2.500000000000000000, 1.178949249685213863, -2.042000000000001148 ) ) ;
#1571 = CARTESIAN_POINT ( 'NONE',  ( 29.50000000000000711, 2.000000000000001776, 2.500000000000000444 ) ) ;
#1572 = ADVANCED_FACE ( 'NONE', ( #10699 ), #2827, .T. ) ;
#1573 = CARTESIAN_POINT ( 'NONE',  ( -0.06616922564517727090, 32.50000000000000711, 13.90844158473306713 ) ) ;
#1574 = DIRECTION ( 'NONE',  ( -1.000000000000000000, -0.000000000000000000, -0.000000000000000000 ) ) ;
#1575 = EDGE_LOOP ( 'NONE', ( #5448, #9550, #1180, #4570 ) ) ;
#1576 = CARTESIAN_POINT ( 'NONE',  ( 2.981723757189247426, 1.693953258775870996, 3.499999999999999112 ) ) ;
#1577 = EDGE_LOOP ( 'NONE', ( #10938, #8661, #3163 ) ) ;
#1578 = ORIENTED_EDGE ( 'NONE', *, *, #9906, .T. ) ;
#1579 = DIRECTION ( 'NONE',  ( 0.000000000000000000, 0.000000000000000000, 1.000000000000000000 ) ) ;
#1580 = CARTESIAN_POINT ( 'NONE',  ( 29.17190429162964094, 2.000000000000001776, -2.500000000000000444 ) ) ;
#1581 = CARTESIAN_POINT ( 'NONE',  ( 20.43380676890320657, 22.25420293214091316, 12.00579112326941988 ) ) ;
#1582 = DIRECTION ( 'NONE',  ( -0.000000000000000000, -0.000000000000000000, -1.000000000000000000 ) ) ;
#1583 = EDGE_CURVE ( 'NONE', #4391, #10481, #4406, .T. ) ;
#1584 = CARTESIAN_POINT ( 'NONE',  ( 34.92403196580097813, 2.306010598194981664, 4.165547504151214220 ) ) ;
#1585 = CARTESIAN_POINT ( 'NONE',  ( -24.35964822603314417, 55.49374999904394912, -5.000000000000103029 ) ) ;
#1586 = EDGE_CURVE ( 'NONE', #10425, #8904, #3201, .T. ) ;
#1587 = CARTESIAN_POINT ( 'NONE',  ( 1.747541505913279281, -3.837784562140273081, -3.503702292528912299 ) ) ;
#1588 = DIRECTION ( 'NONE',  ( -1.000000000000000000, -0.000000000000000000, -0.000000000000000000 ) ) ;
#1589 = ORIENTED_EDGE ( 'NONE', *, *, #9537, .T. ) ;
#1590 = ADVANCED_FACE ( 'NONE', ( #6521 ), #5132, .F. ) ;
#1591 = CARTESIAN_POINT ( 'NONE',  ( -2.500000000000004441, 28.96446609406725159, 14.04687500000000355 ) ) ;
#1592 = LINE ( 'NONE', #10985, #9194 ) ;
#1593 = CARTESIAN_POINT ( 'NONE',  ( -25.98076211353310683, 51.81874999904394485, -3.128098921329806714 ) ) ;
#1594 = EDGE_CURVE ( 'NONE', #2434, #1351, #2285, .T. ) ;
#1595 = CARTESIAN_POINT ( 'NONE',  ( -27.60187600103308725, 54.21041666571061768, -5.935950539335252074 ) ) ;
#1596 = CARTESIAN_POINT ( 'NONE',  ( 18.10462311893278553, 17.05669763433401087, 12.04589798090090902 ) ) ;
#1597 = CARTESIAN_POINT ( 'NONE',  ( -27.98076211353308551, 53.34999999999985931, -5.000000000000103029 ) ) ;
#1598 = VERTEX_POINT ( 'NONE', #2361 ) ;
#1599 = EDGE_CURVE ( 'NONE', #6333, #10496, #326, .T. ) ;
#1600 = EDGE_CURVE ( 'NONE', #4884, #5586, #8535, .T. ) ;
#1601 = FILL_AREA_STYLE_COLOUR ( '', #8306 ) ;
#1602 = ORIENTED_EDGE ( 'NONE', *, *, #7636, .T. ) ;
#1603 = EDGE_LOOP ( 'NONE', ( #4104, #1053, #1842, #4564 ) ) ;
#1604 = CARTESIAN_POINT ( 'NONE',  ( 2.000000000000000000, -1.773042676681341856, 2.276824562219559311E-15 ) ) ;
#1605 = ORIENTED_EDGE ( 'NONE', *, *, #8341, .F. ) ;
#1606 = CARTESIAN_POINT ( 'NONE',  ( -2.500000000000004885, 29.80321974748363090, 16.48359592357600434 ) ) ;
#1607 = EDGE_LOOP ( 'NONE', ( #4800, #10163, #96, #4089, #10341, #4390, #748, #2683, #7548, #10701, #1055 ) ) ;
#1608 = CARTESIAN_POINT ( 'NONE',  ( 19.25788680476432546, 17.21053220311310739, 11.00783986014182148 ) ) ;
#1609 =( NAMED_UNIT ( * ) SI_UNIT ( $, .STERADIAN. ) SOLID_ANGLE_UNIT ( ) );
#1610 = CYLINDRICAL_SURFACE ( 'NONE', #1336, 4.999999999999997335 ) ;
#1611 = CARTESIAN_POINT ( 'NONE',  ( 3.200000000000006839, -3.202582148906703896, 1.452965002680465245 ) ) ;
#1612 = CARTESIAN_POINT ( 'NONE',  ( 24.41364504476855402, 20.99234424618630257, 12.94889058896551326 ) ) ;
#1613 = DIRECTION ( 'NONE',  ( 0.000000000000000000, -0.000000000000000000, 1.000000000000000000 ) ) ;
#1614 = CARTESIAN_POINT ( 'NONE',  ( -26.98076211353309972, 54.54583333142136325, -6.732050807568954909 ) ) ;
#1615 = AXIS2_PLACEMENT_3D ( 'NONE', #1474, #6623, #6692 ) ;
#1616 = CARTESIAN_POINT ( 'NONE',  ( 29.49999999999999289, -3.999999999999993339, 10.00000000000000533 ) ) ;
#1617 = VERTEX_POINT ( 'NONE', #9246 ) ;
#1618 = LINE ( 'NONE', #4347, #4412 ) ;
#1619 = ORIENTED_EDGE ( 'NONE', *, *, #823, .T. ) ;
#1620 = CARTESIAN_POINT ( 'NONE',  ( -1.383578242660661983, 33.52740819067396671, 17.23218341526694530 ) ) ;
#1621 = ORIENTED_EDGE ( 'NONE', *, *, #2893, .F. ) ;
#1622 = EDGE_CURVE ( 'NONE', #2973, #8252, #3368, .T. ) ;
#1623 = CARTESIAN_POINT ( 'NONE',  ( 22.50783536177859645, 18.11075086187001659, 12.94889058896590583 ) ) ;
#1624 = EDGE_CURVE ( 'NONE', #3081, #932, #7240, .T. ) ;
#1625 = VECTOR ( 'NONE', #10324, 999.9999999999998863 ) ;
#1626 = CARTESIAN_POINT ( 'NONE',  ( 22.47621881040483771, 18.15620256126511478, 11.95042449705224819 ) ) ;
#1627 =( BOUNDED_CURVE ( )  B_SPLINE_CURVE ( 2, ( #522, #3090, #10651, #3968, #3764, #4711, #10490, #7202, #5543 ),
 .UNSPECIFIED., .F., .F. ) 
 B_SPLINE_CURVE_WITH_KNOTS ( ( 3, 2, 2, 2, 3 ),
 ( 0.2500000000000000000, 0.2592592592592592449, 0.2777777777777777901, 0.2962962962962962798, 0.3055555555555555802 ),
 .UNSPECIFIED. ) 
 CURVE ( )  GEOMETRIC_REPRESENTATION_ITEM ( )  RATIONAL_B_SPLINE_CURVE ( ( 0.9330127018922192983, 0.9330127018922194093, 1.000000000000000000, 0.8660254037844387076, 1.000000000000000000, 0.8660254037844387076, 1.000000000000000000, 0.9330127018922191873, 0.9330127018922194093 ) ) 
 REPRESENTATION_ITEM ( '' )  );
#1628 = CARTESIAN_POINT ( 'NONE',  ( -24.98076211353213694, 57.99999999999985789, -6.732050807568384698 ) ) ;
#1629 = CARTESIAN_POINT ( 'NONE',  ( 0.000000000000000000, 0.000000000000000000, -0.2800830152838844622 ) ) ;
#1630 = CARTESIAN_POINT ( 'NONE',  ( 1.814555661125942132, 28.27902175519319883, 14.68969158473306535 ) ) ;
#1631 = CARTESIAN_POINT ( 'NONE',  ( 29.49999999999999289, 6.938893903907228378E-15, 17.50000000000000000 ) ) ;
#1632 = DIRECTION ( 'NONE',  ( 4.312387734421997929E-17, -0.7071067811865487940, -0.7071067811865463515 ) ) ;
#1633 = CARTESIAN_POINT ( 'NONE',  ( -25.98076211353311393, 50.28749999808804461, -7.000000000000073719 ) ) ;
#1634 = VERTEX_POINT ( 'NONE', #6749 ) ;
#1635 = ORIENTED_EDGE ( 'NONE', *, *, #7169, .F. ) ;
#1636 = FACE_OUTER_BOUND ( 'NONE', #10823, .T. ) ;
#1637 = CARTESIAN_POINT ( 'NONE',  ( 0.3126073911696503060, 4.041451884327400101, -2.290628625700182053E-14 ) ) ;
#1638 = LINE ( 'NONE', #5034, #10552 ) ;
#1639 = VECTOR ( 'NONE', #6375, 1000.000000000000000 ) ;
#1640 = CARTESIAN_POINT ( 'NONE',  ( -23.98076211353314235, 55.65416666475469754, -3.845299461620867554 ) ) ;
#1641 = DIRECTION ( 'NONE',  ( 0.000000000000000000, 0.000000000000000000, 1.000000000000000000 ) ) ;
#1642 = CARTESIAN_POINT ( 'NONE',  ( -25.17020516978313083, 54.67708333237727913, -3.596074190997380349 ) ) ;
#1643 = CARTESIAN_POINT ( 'NONE',  ( 0.000000000000000000, 30.00000000000000000, 2.500000000000000000 ) ) ;
#1644 = DIRECTION ( 'NONE',  ( 0.000000000000000000, 0.000000000000000000, -1.000000000000000000 ) ) ;
#1645 = ORIENTED_EDGE ( 'NONE', *, *, #1262, .F. ) ;
#1646 = VECTOR ( 'NONE', #2791, 1000.000000000000000 ) ;
#1647 = CARTESIAN_POINT ( 'NONE',  ( -27.98076211353308551, 50.60833333333319928, -3.845299461620869330 ) ) ;
#1648 = DIRECTION ( 'NONE',  ( 1.000000000000000000, -9.251858538542971828E-16, 0.000000000000000000 ) ) ;
#1649 = CARTESIAN_POINT ( 'NONE',  ( -25.98076211353310683, 55.66874999904395338, -6.871901078670399343 ) ) ;
#1650 = CARTESIAN_POINT ( 'NONE',  ( -24.35964822603314772, 51.76041666571061484, -4.064049460664953983 ) ) ;
#1651 = DIRECTION ( 'NONE',  ( 0.000000000000000000, 0.000000000000000000, 1.000000000000000000 ) ) ;
#1652 = CARTESIAN_POINT ( 'NONE',  ( -24.98076211353312814, 53.81666666666652787, -6.732050807568954909 ) ) ;
#1653 = ORIENTED_EDGE ( 'NONE', *, *, #10884, .F. ) ;
#1654 = EDGE_CURVE ( 'NONE', #10106, #7739, #2707, .T. ) ;
#1655 = ORIENTED_EDGE ( 'NONE', *, *, #4757, .T. ) ;
#1656 = ORIENTED_EDGE ( 'NONE', *, *, #3408, .F. ) ;
#1657 = DIRECTION ( 'NONE',  ( 0.000000000000000000, -1.000000000000000000, 0.000000000000000000 ) ) ;
#1659 = ORIENTED_EDGE ( 'NONE', *, *, #8430, .F. ) ;
#1658 = ADVANCED_FACE ( 'NONE', ( #8477 ), #2108, .T. ) ;
#1660 = FACE_OUTER_BOUND ( 'NONE', #9991, .T. ) ;
#1661 = DIRECTION ( 'NONE',  ( -1.368128411675317953E-17, 3.330669073875469621E-16, -1.000000000000000222 ) ) ;
#1662 = VERTEX_POINT ( 'NONE', #796 ) ;
#1663 = CARTESIAN_POINT ( 'NONE',  ( 22.00433854689477897, 19.11167697002443333, 11.00732503135576401 ) ) ;
#1664 = DIRECTION ( 'NONE',  ( -1.000000000000000000, -6.098637220230963674E-17, 0.000000000000000000 ) ) ;
#1665 = CARTESIAN_POINT ( 'NONE',  ( 25.00000000000000000, 0.000000000000000000, 0.000000000000000000 ) ) ;
#1666 = CARTESIAN_POINT ( 'NONE',  ( -26.79131905728310059, 50.12708333237728198, -6.403925809002825709 ) ) ;
#1667 = CARTESIAN_POINT ( 'NONE',  ( 22.43871220627207563, 23.52649944903870249, 11.95042449705224819 ) ) ;
#1668 = CARTESIAN_POINT ( 'NONE',  ( 4.000000000000000000, 0.3987449864460005378, -0.01220643443059817035 ) ) ;
#1669 = CARTESIAN_POINT ( 'NONE',  ( -27.78269016046133544, 56.11211611946337285, -4.132212402892765368 ) ) ;
#1670 = DIRECTION ( 'NONE',  ( -1.000000000000000000, -6.098637220230963674E-17, -1.156482317317871725E-16 ) ) ;
#1671 = ORIENTED_EDGE ( 'NONE', *, *, #9189, .F. ) ;
#1672 = CARTESIAN_POINT ( 'NONE',  ( -24.98076211353193798, 57.99999999999910472, -3.267949192431741423 ) ) ;
#1673 = ORIENTED_EDGE ( 'NONE', *, *, #2965, .T. ) ;
#1674 = CARTESIAN_POINT ( 'NONE',  ( 3.527408190673962274, 28.61642175733934934, 14.76781658473306535 ) ) ;
#1675 = ORIENTED_EDGE ( 'NONE', *, *, #4069, .F. ) ;
#1676 = CARTESIAN_POINT ( 'NONE',  ( 23.01143949934618504, 18.46103507366711227, 12.94889058896576906 ) ) ;
#1677 = AXIS2_PLACEMENT_3D ( 'NONE', #4954, #10878, #3266 ) ;
#1678 = DIRECTION ( 'NONE',  ( 0.000000000000000000, 0.000000000000000000, 1.000000000000000000 ) ) ;
#1679 = CARTESIAN_POINT ( 'NONE',  ( -25.98076211353311393, 51.68749999808803608, -7.000000000000073719 ) ) ;
#1680 = CARTESIAN_POINT ( 'NONE',  ( -25.98076211353311393, 51.64374999904395480, -3.128098921329806714 ) ) ;
#1681 = STYLED_ITEM ( 'NONE', ( #3272 ), #9072 ) ;
#1682 = VECTOR ( 'NONE', #1012, 1000.000000000000000 ) ;
#1683 = CARTESIAN_POINT ( 'NONE',  ( 2.472591809326049272, 31.10170313157791711, 14.92406658473306713 ) ) ;
#1684 = PLANE ( 'NONE',  #1709 ) ;
#1685 = CARTESIAN_POINT ( 'NONE',  ( -31.74999999999995737, 0.000000000000000000, 0.000000000000000000 ) ) ;
#1686 = CARTESIAN_POINT ( 'NONE',  ( 29.49999999999999645, -3.999999999999983569, 8.350000000000013856 ) ) ;
#1687 = VERTEX_POINT ( 'NONE', #5154 ) ;
#1688 = EDGE_LOOP ( 'NONE', ( #8283, #1534, #3204, #10954, #9953 ) ) ;
#1689 = ADVANCED_FACE ( 'NONE', ( #4201 ), #10919, .T. ) ;
#1690 = CARTESIAN_POINT ( 'NONE',  ( -25.71106610644865498, 16.50000000000026290, -5.000000000000000000 ) ) ;
#1691 = VECTOR ( 'NONE', #89, 1000.000000000000000 ) ;
#1692 = FACE_OUTER_BOUND ( 'NONE', #531, .T. ) ;
#1693 = CIRCLE ( 'NONE', #7367, 4.500000000000000000 ) ;
#1694 = CARTESIAN_POINT ( 'NONE',  ( 22.29575558078030895, 19.24694448270711788, 12.00579112326941988 ) ) ;
#1695 = CONICAL_SURFACE ( 'NONE', #2228, 1.649999999999998579, 1.029744258676653423 ) ;
#1696 = CARTESIAN_POINT ( 'NONE',  ( 2.500000000000008438, 30.00000000000000711, 15.84375000000000355 ) ) ;
#1697 = DIRECTION ( 'NONE',  ( 1.000000000000000000, 0.000000000000000000, 0.000000000000000000 ) ) ;
#1698 = CARTESIAN_POINT ( 'NONE',  ( -26.79131905728310059, 52.75208333237728198, -6.403925809002825709 ) ) ;
#1699 = CARTESIAN_POINT ( 'NONE',  ( 2.000000000000000000, -1.773042676681341856, 2.276824562219559311E-15 ) ) ;
#1700 = CARTESIAN_POINT ( 'NONE',  ( 0.000000000000000000, 0.000000000000000000, 2.500000000000000000 ) ) ;
#1701 = CARTESIAN_POINT ( 'NONE',  ( 0.000000000000000000, 0.000000000000000000, 2.500000000000000000 ) ) ;
#1702 = VECTOR ( 'NONE', #2138, 1000.000000000000000 ) ;
#1703 = VERTEX_POINT ( 'NONE', #4984 ) ;
#1704 = AXIS2_PLACEMENT_3D ( 'NONE', #8983, #9925, #2106 ) ;
#1705 = DIRECTION ( 'NONE',  ( -2.775557561562891351E-17, -1.000000000000000000, 8.326672684688671588E-17 ) ) ;
#1706 = CARTESIAN_POINT ( 'NONE',  ( 2.000000000000000000, -0.8865213383406694847, 1.535500000000001419 ) ) ;
#1707 = CARTESIAN_POINT ( 'NONE',  ( -24.35964822603314772, 54.03541666571062052, -4.064049460664953983 ) ) ;
#1708 = CARTESIAN_POINT ( 'NONE',  ( 29.49999999999999645, -3.999999999999983569, 11.64999999999999858 ) ) ;
#1709 = AXIS2_PLACEMENT_3D ( 'NONE', #1631, #10902, #8291 ) ;
#1710 = DIRECTION ( 'NONE',  ( 0.000000000000000000, 0.000000000000000000, -1.000000000000000000 ) ) ;
#1711 = CARTESIAN_POINT ( 'NONE',  ( -27.98076211353308551, 54.04999999999986215, -5.000000000000103029 ) ) ;
#1712 = ORIENTED_EDGE ( 'NONE', *, *, #5400, .T. ) ;
#1713 = EDGE_CURVE ( 'NONE', #3725, #4079, #1758, .T. ) ;
#1714 = ORIENTED_EDGE ( 'NONE', *, *, #749, .F. ) ;
#1715 = VERTEX_POINT ( 'NONE', #10980 ) ;
#1716 = FACE_OUTER_BOUND ( 'NONE', #7064, .T. ) ;
#1717 = VERTEX_POINT ( 'NONE', #8358 ) ;
#1718 = CARTESIAN_POINT ( 'NONE',  ( 0.000000000000000000, 30.00000000000000000, -2.499999999999998668 ) ) ;
#1719 = ORIENTED_EDGE ( 'NONE', *, *, #3774, .T. ) ;
#1720 = CARTESIAN_POINT ( 'NONE',  ( 21.25655365073496839, 18.52406763439849513, 12.00579112326941988 ) ) ;
#1721 = CARTESIAN_POINT ( 'NONE',  ( 0.000000000000000000, 30.00000000000000000, -2.500000000000000000 ) ) ;
#1722 = CARTESIAN_POINT ( 'NONE',  ( -25.98076211353311393, 55.18749999808803608, -7.000000000000072831 ) ) ;
#1723 = ORIENTED_EDGE ( 'NONE', *, *, #9806, .T. ) ;
#1724 = CARTESIAN_POINT ( 'NONE',  ( 2.000000000000000000, -0.8865213383406694847, 1.535500000000001419 ) ) ;
#1725 = ADVANCED_FACE ( 'NONE', ( #10146 ), #1763, .T. ) ;
#1726 = CARTESIAN_POINT ( 'NONE',  ( 21.01569960522067504, 17.20769859423666048, 10.95195840513859231 ) ) ;
#1727 = FACE_OUTER_BOUND ( 'NONE', #10304, .T. ) ;
#1728 = B_SPLINE_CURVE_WITH_KNOTS ( 'NONE', 3,
 ( #2309, #4026, #5700, #4198, #6572 ),
 .UNSPECIFIED., .F., .F.,
 ( 4, 1, 4 ),
 ( 0.000000000000000000, 0.002309401076758505790, 0.004618802153517011580 ),
 .UNSPECIFIED. ) ;
#1729 = EDGE_CURVE ( 'NONE', #590, #6915, #9910, .T. ) ;
#1730 = CARTESIAN_POINT ( 'NONE',  ( -25.17020516978313083, 50.71041666571061057, -6.403925809002825709 ) ) ;
#1731 = DIRECTION ( 'NONE',  ( -1.000000000000000000, -6.098637220230963674E-17, -1.156482317317871725E-16 ) ) ;
#1732 = ORIENTED_EDGE ( 'NONE', *, *, #2433, .T. ) ;
#1733 = LINE ( 'NONE', #10949, #4942 ) ;
#1734 = ORIENTED_EDGE ( 'NONE', *, *, #10284, .F. ) ;
#1735 = CIRCLE ( 'NONE', #10951, 4.000000000000000000 ) ;
#1736 = AXIS2_PLACEMENT_3D ( 'NONE', #10463, #5458, #8733 ) ;
#1737 = CARTESIAN_POINT ( 'NONE',  ( -3.446545381698513655, 29.38705359262400663, 15.50141270685246830 ) ) ;
#1738 = VERTEX_POINT ( 'NONE', #4261 ) ;
#1739 = CARTESIAN_POINT ( 'NONE',  ( 20.19688095354152324, 19.67517542290917731, 13.00425721518307753 ) ) ;
#1740 = EDGE_CURVE ( 'NONE', #8489, #6512, #6695, .T. ) ;
#1741 = LINE ( 'NONE', #8396, #7743 ) ;
#1742 = AXIS2_PLACEMENT_3D ( 'NONE', #10521, #1970, #10468 ) ;
#1743 =( GEOMETRIC_REPRESENTATION_CONTEXT ( 3 ) GLOBAL_UNCERTAINTY_ASSIGNED_CONTEXT ( ( #9535 ) ) GLOBAL_UNIT_ASSIGNED_CONTEXT ( ( #5567, #3731, #4682 ) ) REPRESENTATION_CONTEXT ( 'NONE', 'WORKASPACE' ) );
#1744 = CARTESIAN_POINT ( 'NONE',  ( 21.05771646464872404, 22.57981893131178452, 12.00579112326941988 ) ) ;
#1745 = DIRECTION ( 'NONE',  ( 0.000000000000000000, 0.000000000000000000, -1.000000000000000000 ) ) ;
#1746 = CARTESIAN_POINT ( 'NONE',  ( -1.767766952966375094, 31.76776695296636888, 16.31250000000000355 ) ) ;
#1747 = DIRECTION ( 'NONE',  ( 1.000000000000000000, 0.000000000000000000, 0.000000000000000000 ) ) ;
#1748 = FACE_OUTER_BOUND ( 'NONE', #10082, .T. ) ;
#1749 = CARTESIAN_POINT ( 'NONE',  ( -26.97398308763695596, 58.13372405103771001, -6.736012309356057770 ) ) ;
#1750 = APPLICATION_CONTEXT ( 'automotive_design' ) ;
#1751 = ADVANCED_FACE ( 'NONE', ( #10091 ), #2481, .T. ) ;
#1752 = EDGE_LOOP ( 'NONE', ( #3263, #10095, #7264 ) ) ;
#1753 = ADVANCED_FACE ( 'NONE', ( #4316 ), #5917, .T. ) ;
#1754 = ORIENTED_EDGE ( 'NONE', *, *, #10410, .F. ) ;
#1755 = CONICAL_SURFACE ( 'NONE', #9374, 4.624785217660733139, 1.047197551196604071 ) ;
#1756 =( GEOMETRIC_REPRESENTATION_CONTEXT ( 3 ) GLOBAL_UNCERTAINTY_ASSIGNED_CONTEXT ( ( #10432 ) ) GLOBAL_UNIT_ASSIGNED_CONTEXT ( ( #7554, #3333, #1495 ) ) REPRESENTATION_CONTEXT ( 'NONE', 'WORKASPACE' ) );
#1757 = CARTESIAN_POINT ( 'NONE',  ( -25.98076211353311393, 49.49999999999986500, -3.000000000000131894 ) ) ;
#1758 = CIRCLE ( 'NONE', #4421, 3.500000000000000000 ) ;
#1759 = CARTESIAN_POINT ( 'NONE',  ( 22.03595509826854126, 19.06622527062933870, 12.00579112326941988 ) ) ;
#1760 = CARTESIAN_POINT ( 'NONE',  ( 2.500000000000008438, 30.00000000000000711, 14.59375000000000178 ) ) ;
#1761 = DIRECTION ( 'NONE',  ( 0.000000000000000000, -0.5000000000000012212, -0.8660254037844380415 ) ) ;
#1762 = CARTESIAN_POINT ( 'NONE',  ( -27.60187600103308014, 54.91041666571061342, -5.935950539335252074 ) ) ;
#1763 = PLANE ( 'NONE',  #7963 ) ;
#1764 = DIRECTION ( 'NONE',  ( 0.000000000000000000, 2.312964634635742464E-16, 1.000000000000000000 ) ) ;
#1765 = DIRECTION ( 'NONE',  ( -1.000000000000000000, -6.098637220230963674E-17, 0.000000000000000000 ) ) ;
#1766 = ORIENTED_EDGE ( 'NONE', *, *, #2279, .F. ) ;
#1767 = LINE ( 'NONE', #917, #7339 ) ;
#1768 = CARTESIAN_POINT ( 'NONE',  ( 1.567478505476134606E-15, 4.618802153517012066, -3.433295621305382905 ) ) ;
#1769 = EDGE_CURVE ( 'NONE', #4847, #3729, #24, .T. ) ;
#1770 = CARTESIAN_POINT ( 'NONE',  ( -24.35964822603314417, 53.39374999904394770, -5.000000000000103029 ) ) ;
#1771 = CARTESIAN_POINT ( 'NONE',  ( 0.000000000000000000, -1.773042676681341856, 2.276824562219559311E-15 ) ) ;
#1772 = LINE ( 'NONE', #3549, #9979 ) ;
#1773 = CARTESIAN_POINT ( 'NONE',  ( -27.98076211353308551, 50.60833333333320638, -3.845299461620869330 ) ) ;
#1774 = EDGE_LOOP ( 'NONE', ( #3839, #9318, #3581, #10119, #9490, #6576 ) ) ;
#1775 = ORIENTED_EDGE ( 'NONE', *, *, #5684, .F. ) ;
#1776 = CARTESIAN_POINT ( 'NONE',  ( 0.000000000000000000, 0.000000000000000000, -3.499999999999999556 ) ) ;
#1777 = MANIFOLD_SOLID_BREP ( 'DomeFillet', #10014 ) ;
#1778 = DIRECTION ( 'NONE',  ( -0.000000000000000000, -0.000000000000000000, 1.000000000000000000 ) ) ;
#1779 = APPLICATION_PROTOCOL_DEFINITION ( 'draft international standard', 'automotive_design', 1998, #2307 ) ;
#1780 = ORIENTED_EDGE ( 'NONE', *, *, #8238, .F. ) ;
#1781 = CARTESIAN_POINT ( 'NONE',  ( 20.08745147943499987, 17.71083118005251933, 12.00579112326941988 ) ) ;
#1782 = FACE_OUTER_BOUND ( 'NONE', #1603, .T. ) ;
#1783 = EDGE_CURVE ( 'NONE', #8322, #7952, #9375, .T. ) ;
#1784 = DIRECTION ( 'NONE',  ( 0.000000000000000000, 0.000000000000000000, -1.000000000000000000 ) ) ;
#1785 = DIRECTION ( 'NONE',  ( -2.775557561562891351E-17, -1.000000000000000000, 8.326672684688671588E-17 ) ) ;
#1786 = CARTESIAN_POINT ( 'NONE',  ( 19.38445574543743177, 22.63941596627307362, 11.95042449705263898 ) ) ;
#1787 = CARTESIAN_POINT ( 'NONE',  ( 3.500000000000005329, 30.00000000000000000, 15.84375000000000355 ) ) ;
#1788 = CARTESIAN_POINT ( 'NONE',  ( -27.98076211353308551, 53.90416666475469754, -6.154700538379338504 ) ) ;
#1789 = DIRECTION ( 'NONE',  ( 0.000000000000000000, 0.000000000000000000, 1.000000000000000000 ) ) ;
#1790 = ORIENTED_EDGE ( 'NONE', *, *, #7191, .F. ) ;
#1791 = DIRECTION ( 'NONE',  ( 4.312387734421997313E-17, -0.7071067811865486830, -0.7071067811865463515 ) ) ;
#1792 = ORIENTED_EDGE ( 'NONE', *, *, #4130, .F. ) ;
#1793 = CARTESIAN_POINT ( 'NONE',  ( -3.472591809326043499, 28.48408330604899064, 13.04906658473306891 ) ) ;
#1794 = ORIENTED_EDGE ( 'NONE', *, *, #3531, .F. ) ;
#1795 = CARTESIAN_POINT ( 'NONE',  ( 16.72700999897183038, 16.80849948458634557, 12.09707671258119888 ) ) ;
#1796 = EDGE_CURVE ( 'NONE', #8872, #5599, #7668, .T. ) ;
#1797 = EDGE_CURVE ( 'NONE', #2436, #2510, #1024, .T. ) ;
#1798 = CARTESIAN_POINT ( 'NONE',  ( 17.78598590678423719, 16.10215687441832699, 12.01726674494117653 ) ) ;
#1799 = CARTESIAN_POINT ( 'NONE',  ( 20.23853826540680600, 19.71164639310234534, 12.00579112326941988 ) ) ;
#1800 = FACE_OUTER_BOUND ( 'NONE', #3769, .T. ) ;
#1801 = CARTESIAN_POINT ( 'NONE',  ( -2.469212770973128190, 29.60886282244813117, 16.49922112211940117 ) ) ;
#1802 = LINE ( 'NONE', #5519, #9494 ) ;
#1803 = CARTESIAN_POINT ( 'NONE',  ( -26.59672572989580175, 58.79818731520758490, -6.905264038683467831 ) ) ;
#1804 = VERTEX_POINT ( 'NONE', #6362 ) ;
#1805 = EDGE_CURVE ( 'NONE', #10564, #183, #7190, .T. ) ;
#1806 = ORIENTED_EDGE ( 'NONE', *, *, #6807, .F. ) ;
#1807 = ADVANCED_FACE ( 'NONE', ( #10422 ), #2983, .F. ) ;
#1808 = CARTESIAN_POINT ( 'NONE',  ( 1.734723475976807094E-15, 4.618802153517012954, -0.4999999999999995559 ) ) ;
#1809 = CARTESIAN_POINT ( 'NONE',  ( -4.000000000000000000, -2.472261339043343220, -3.687027428081192326 ) ) ;
#1810 = CARTESIAN_POINT ( 'NONE',  ( -2.688821387764050996E-14, -4.618802153517012954, -0.4999999999999995559 ) ) ;
#1811 = FACE_OUTER_BOUND ( 'NONE', #527, .T. ) ;
#1812 = CARTESIAN_POINT ( 'NONE',  ( -25.17020516978313083, 53.10208333237728340, -3.596074190997380349 ) ) ;
#1813 = CARTESIAN_POINT ( 'NONE',  ( -25.98076211353311393, 49.49999999999986500, -3.000000000000131894 ) ) ;
#1814 = CARTESIAN_POINT ( 'NONE',  ( 2.548804901056335857E-15, 4.736522675502163437, -3.681124513963624612 ) ) ;
#1815 = LINE ( 'NONE', #7089, #3829 ) ;
#1816 = ORIENTED_EDGE ( 'NONE', *, *, #10153, .F. ) ;
#1817 = DIRECTION ( 'NONE',  ( 0.000000000000000000, -0.000000000000000000, -1.000000000000000000 ) ) ;
#1818 = CARTESIAN_POINT ( 'NONE',  ( -1.767766952966375094, 31.76776695296636888, 16.31250000000000355 ) ) ;
#1819 = CARTESIAN_POINT ( 'NONE',  ( -0.6666666666666651864, 4.233901974057260098, -3.300726591567081147 ) ) ;
#1820 = CARTESIAN_POINT ( 'NONE',  ( -27.60187600103308725, 55.08541666571062478, -5.935950539335252074 ) ) ;
#1821 = CARTESIAN_POINT ( 'NONE',  ( 29.49999999999999645, 2.000000000000001776, -12.49999999999999822 ) ) ;
#1822 = PRODUCT_DEFINITION_SHAPE ( 'NONE', 'NONE',  #10999 ) ;
#1823 = CARTESIAN_POINT ( 'NONE',  ( 30.75045812061784289, 56.49999999999984368, 14.50000000000000000 ) ) ;
#1824 = CARTESIAN_POINT ( 'NONE',  ( -25.98076211353311393, 49.49999999999986500, -5.000000000000103029 ) ) ;
#1825 = CIRCLE ( 'NONE', #1100, 2.500000000000000444 ) ;
#1826 = ORIENTED_EDGE ( 'NONE', *, *, #8639, .T. ) ;
#1827 = ORIENTED_EDGE ( 'NONE', *, *, #10610, .T. ) ;
#1828 = CARTESIAN_POINT ( 'NONE',  ( 2.500000000000000000, -1.178949249685213863, 2.042000000000002924 ) ) ;
#1829 = CARTESIAN_POINT ( 'NONE',  ( 0.1999999999999987899, 0.000000000000000000, 3.299999999999999822 ) ) ;
#1830 = APPLICATION_PROTOCOL_DEFINITION ( 'draft international standard', 'automotive_design', 1998, #2888 ) ;
#1831 = EDGE_LOOP ( 'NONE', ( #6646, #1826, #784, #612, #9485, #3243, #4119, #8001, #943, #9944, #8294, #9926, #3834, #945, #700, #871, #8492, #2455, #6586, #5020, #1905 ) ) ;
#1832 = EDGE_CURVE ( 'NONE', #7103, #7090, #1076, .T. ) ;
#1833 = DIRECTION ( 'NONE',  ( 0.000000000000000000, 0.000000000000000000, -1.000000000000000000 ) ) ;
#1834 = DIRECTION ( 'NONE',  ( 1.000000000000000000, 0.000000000000000000, 0.000000000000000000 ) ) ;
#1835 = CARTESIAN_POINT ( 'NONE',  ( 34.64101615137754919, 5.000000000000002665, -2.500000000000000000 ) ) ;
#1836 = CARTESIAN_POINT ( 'NONE',  ( 20.26791470906062997, 16.62008925861079334, 11.95042449705224819 ) ) ;
#1837 = FACE_OUTER_BOUND ( 'NONE', #2647, .T. ) ;
#1838 = CARTESIAN_POINT ( 'NONE',  ( -26.98076211353309972, 55.94583333142136894, -6.732050807568954909 ) ) ;
#1839 = CARTESIAN_POINT ( 'NONE',  ( -4.000000000000000000, 2.309401076758498483, -5.000000000000000000 ) ) ;
#1840 = VERTEX_POINT ( 'NONE', #8643 ) ;
#1841 = FACE_OUTER_BOUND ( 'NONE', #10523, .T. ) ;
#1842 = ORIENTED_EDGE ( 'NONE', *, *, #524, .F. ) ;
#1843 = CARTESIAN_POINT ( 'NONE',  ( 3.500000000000003997, 30.06616922564517580, 14.84594158473306713 ) ) ;
#1844 = EDGE_LOOP ( 'NONE', ( #5665, #3253, #8856, #1996 ) ) ;
#1845 = CARTESIAN_POINT ( 'NONE',  ( 19.76265562249496099, 16.28401831655332543, 11.95127577209155234 ) ) ;
#1846 = MANIFOLD_SOLID_BREP ( 'Cut-Extrude1', #8957 ) ;
#1847 = CARTESIAN_POINT ( 'NONE',  ( -25.71518008040301240, 58.97299622964627730, -6.986129658743783999 ) ) ;
#1848 = DIRECTION ( 'NONE',  ( 0.000000000000000000, 0.000000000000000000, 1.000000000000000000 ) ) ;
#1849 = CARTESIAN_POINT ( 'NONE',  ( -25.98076211353311393, 50.94374999904395196, -3.128098921329806714 ) ) ;
#1850 = CARTESIAN_POINT ( 'NONE',  ( 1.035533905932743970, 27.49999999999999289, 15.60937500000000711 ) ) ;
#1851 = LINE ( 'NONE', #955, #975 ) ;
#1852 = DIRECTION ( 'NONE',  ( 0.000000000000000000, 1.000000000000000000, 0.000000000000000000 ) ) ;
#1853 = EDGE_CURVE ( 'NONE', #7739, #625, #9635, .T. ) ;
#1854 = ORIENTED_EDGE ( 'NONE', *, *, #4757, .F. ) ;
#1855 = ORIENTED_EDGE ( 'NONE', *, *, #7793, .F. ) ;
#1856 = VECTOR ( 'NONE', #29, 1000.000000000000000 ) ;
#1857 = LINE ( 'NONE', #132, #6662 ) ;
#1858 = DIRECTION ( 'NONE',  ( 0.000000000000000000, 1.000000000000000000, 0.000000000000000000 ) ) ;
#1859 = VECTOR ( 'NONE', #10695, 1000.000000000000000 ) ;
#1860 = CARTESIAN_POINT ( 'NONE',  ( -2.469212770973128190, 29.60886282244813827, 16.49922112211940117 ) ) ;
#1861 = CLOSED_SHELL ( 'NONE', ( #6431, #3852, #7424, #5521, #979, #7108, #8371, #10145, #9876, #9253, #7257, #3375, #1101, #9150, #3232, #771, #3744, #9256, #7361, #5940, #5339, #8158, #10303, #3290, #4867, #4724, #1416 ) ) ;
#1862 = LINE ( 'NONE', #7700, #3214 ) ;
#1863 = CARTESIAN_POINT ( 'NONE',  ( -26.79131905728310059, 54.38541666571061484, -3.596074190997381237 ) ) ;
#1864 = AXIS2_PLACEMENT_3D ( 'NONE', #4452, #5383, #3772 ) ;
#1865 = ADVANCED_FACE ( 'NONE', ( #1189, #7978 ), #2090, .F. ) ;
#1866 = PLANE ( 'NONE',  #3983 ) ;
#1867 = CARTESIAN_POINT ( 'NONE',  ( 2.855764796983346177, -2.970025579236428737, -0.09382832055446485575 ) ) ;
#1868 = ORIENTED_EDGE ( 'NONE', *, *, #3317, .T. ) ;
#1869 =( NAMED_UNIT ( * ) SI_UNIT ( $, .STERADIAN. ) SOLID_ANGLE_UNIT ( ) );
#1870 = AXIS2_PLACEMENT_3D ( 'NONE', #8610, #7727, #1895 ) ;
#1871 = CARTESIAN_POINT ( 'NONE',  ( 2.500000000000009770, 29.93383077435482420, 16.84155841526694175 ) ) ;
#1872 = VECTOR ( 'NONE', #7281, 1000.000000000000000 ) ;
#1873 = CARTESIAN_POINT ( 'NONE',  ( 4.211140560182196957, -2.431303136016555122, -3.745885042887436622 ) ) ;
#1874 =( BOUNDED_SURFACE ( )  B_SPLINE_SURFACE ( 3, 2, ( 
 ( #4842, #8216, #5570 ),
 ( #2287, #9948, #7387 ),
 ( #1499, #3064, #8898 ),
 ( #3842, #5675, #4900 ),
 ( #8169, #6393, #3997 ),
 ( #10778, #3167, #9053 ) ),
 .UNSPECIFIED., .F., .F., .F. ) 
 B_SPLINE_SURFACE_WITH_KNOTS ( ( 4, 2, 4 ),
 ( 3, 3 ),
 ( 0.02032853247518126918, 0.02278863295364821906, 0.02524873343211517240 ),
 ( 0.000000000000000000, 1.000000000000000000 ),
 .UNSPECIFIED. ) 
 GEOMETRIC_REPRESENTATION_ITEM ( )  RATIONAL_B_SPLINE_SURFACE ( (
 ( 1.000000000000000000, 0.8047781615896837382, 1.000000000000000000),
 ( 1.000000000000000000, 0.8123767586289252218, 1.000000000000000000),
 ( 1.000000000000000000, 0.8190662415564388121, 1.000000000000000000),
 ( 1.000000000000000000, 0.8192361015669026303, 1.000000000000000000),
 ( 1.000000000000000000, 0.8126135807103900266, 1.000000000000000000),
 ( 1.000000000000000000, 0.8047712338318593339, 1.000000000000000000) ) ) 
 REPRESENTATION_ITEM ( '' )  SURFACE ( )  );
#1875 = UNCERTAINTY_MEASURE_WITH_UNIT (LENGTH_MEASURE( 1.000000000000000082E-05 ), #4788, 'distance_accuracy_value', 'NONE');
#1876 = AXIS2_PLACEMENT_3D ( 'NONE', #8470, #8578, #961 ) ;
#1877 = VECTOR ( 'NONE', #4617, 1000.000000000000000 ) ;
#1878 = CARTESIAN_POINT ( 'NONE',  ( -26.79131905728310059, 53.16041666571061342, -3.596074190997381237 ) ) ;
#1879 = CARTESIAN_POINT ( 'NONE',  ( -27.60187600103308370, 55.66874999904394627, -5.000000000000103029 ) ) ;
#1880 = ADVANCED_FACE ( 'NONE', ( #10685 ), #2459, .T. ) ;
#1881 = VECTOR ( 'NONE', #6571, 1000.000000000000114 ) ;
#1882 = CARTESIAN_POINT ( 'NONE',  ( 34.99999999999999289, 2.000000000000002220, 17.50000000000000355 ) ) ;
#1883 = CARTESIAN_POINT ( 'NONE',  ( -27.98076211353308196, 55.47306177707831409, -4.543495204426306167 ) ) ;
#1884 = AXIS2_PLACEMENT_3D ( 'NONE', #10480, #970, #6865 ) ;
#1885 = ORIENTED_EDGE ( 'NONE', *, *, #5967, .F. ) ;
#1886 = ORIENTED_EDGE ( 'NONE', *, *, #10803, .T. ) ;
#1887 = CYLINDRICAL_SURFACE ( 'NONE', #10365, 1.999999999999971356 ) ;
#1888 = EDGE_CURVE ( 'NONE', #9170, #5606, #1345, .T. ) ;
#1889 = FACE_OUTER_BOUND ( 'NONE', #6739, .T. ) ;
#1890 = PRODUCT_CONTEXT ( 'NONE', #3230, 'mechanical' ) ;
#1891 = ORIENTED_EDGE ( 'NONE', *, *, #5988, .F. ) ;
#1892 = PLANE ( 'NONE',  #4534 ) ;
#1893 = AXIS2_PLACEMENT_3D ( 'NONE', #10249, #731, #2411 ) ;
#1894 = B_SPLINE_CURVE_WITH_KNOTS ( 'NONE', 3,
 ( #1164, #7114, #432, #1227, #3835, #2008 ),
 .UNSPECIFIED., .F., .F.,
 ( 4, 2, 4 ),
 ( 0.003657268138676071038, 0.004679653797516804964, 0.005702039456357537589 ),
 .UNSPECIFIED. ) ;
#1895 = DIRECTION ( 'NONE',  ( 0.000000000000000000, -0.4999999999999992784, 0.8660254037844389297 ) ) ;
#1896 =( REPRESENTATION_RELATIONSHIP ('NONE','NONE', #7540, #716 ) REPRESENTATION_RELATIONSHIP_WITH_TRANSFORMATION ( #4826 )SHAPE_REPRESENTATION_RELATIONSHIP( ) );
#1897 = CARTESIAN_POINT ( 'NONE',  ( 18.60991190964745456, 16.01828113007465504, 10.97873183052796620 ) ) ;
#1898 = EDGE_CURVE ( 'NONE', #8716, #10904, #763, .T. ) ;
#1899 = DIRECTION ( 'NONE',  ( -1.000000000000000000, -0.000000000000000000, -0.000000000000000000 ) ) ;
#1900 = CARTESIAN_POINT ( 'NONE',  ( -26.79131905728310059, 53.16041666571061342, -3.596074190997381237 ) ) ;
#1901 = DIRECTION ( 'NONE',  ( -0.8660254037844401509, 0.4999999999999974465, 0.000000000000000000 ) ) ;
#1902 = ORIENTED_EDGE ( 'NONE', *, *, #2908, .T. ) ;
#1903 = CARTESIAN_POINT ( 'NONE',  ( -2.649999999999991029, 30.00000000000000000, -2.500000000000000000 ) ) ;
#1904 = AXIS2_PLACEMENT_3D ( 'NONE', #7251, #569, #9127 ) ;
#1905 = ORIENTED_EDGE ( 'NONE', *, *, #293, .F. ) ;
#1906 = CARTESIAN_POINT ( 'NONE',  ( -1.734723475976807094E-15, 33.50000000000000000, 16.15625000000000355 ) ) ;
#1907 = VERTEX_POINT ( 'NONE', #2450 ) ;
#1908 = CARTESIAN_POINT ( 'NONE',  ( 18.07012887690021330, 16.02595819568259827, 12.00212024154935975 ) ) ;
#1909 = FILL_AREA_STYLE ('',( #10293 ) ) ;
#1910 = MANIFOLD_SOLID_BREP ( 'Hex', #1861 ) ;
#1911 = DIRECTION ( 'NONE',  ( 0.000000000000000000, 0.000000000000000000, -1.000000000000000000 ) ) ;
#1912 = LINE ( 'NONE', #7745, #5203 ) ;
#1913 = CARTESIAN_POINT ( 'NONE',  ( 29.50000000000000711, -7.999999999999996447, -12.50000000000000000 ) ) ;
#1914 = DIRECTION ( 'NONE',  ( 0.000000000000000000, 0.000000000000000000, 1.000000000000000000 ) ) ;
#1915 = CARTESIAN_POINT ( 'NONE',  ( 24.49999999999999289, -8.499999999999985789, -4.999999999999992006 ) ) ;
#1916 = DIRECTION ( 'NONE',  ( -1.000000000000000000, 0.000000000000000000, 0.000000000000000000 ) ) ;
#1917 = ORIENTED_EDGE ( 'NONE', *, *, #7627, .F. ) ;
#1918 = EDGE_LOOP ( 'NONE', ( #10991, #6008, #3805, #6399 ) ) ;
#1919 = PLANE ( 'NONE',  #4194 ) ;
#1920 = DIRECTION ( 'NONE',  ( 0.000000000000000000, 0.000000000000000000, 1.000000000000000000 ) ) ;
#1921 = AXIS2_PLACEMENT_3D ( 'NONE', #5520, #8065, #8955 ) ;
#1922 = VECTOR ( 'NONE', #1785, 1000.000000000000000 ) ;
#1923 = PLANE ( 'NONE',  #7910 ) ;
#1924 = EDGE_CURVE ( 'NONE', #7431, #7847, #4956, .T. ) ;
#1925 = CARTESIAN_POINT ( 'NONE',  ( -26.48997544305390051, 58.87073604165634322, -3.061924168864667894 ) ) ;
#1926 = CARTESIAN_POINT ( 'NONE',  ( 3.540020015735602765, 2.810662092924382627, -3.602146406945867962 ) ) ;
#1927 = CARTESIAN_POINT ( 'NONE',  ( -25.17020516978313083, 52.40208333237728766, -3.596074190997380349 ) ) ;
#1928 = FILL_AREA_STYLE ('',( #2820 ) ) ;
#1929 = DIRECTION ( 'NONE',  ( -1.000000000000000000, -6.098637220230963674E-17, -1.156482317317871478E-16 ) ) ;
#1930 = CARTESIAN_POINT ( 'NONE',  ( -21.21106610644865498, 16.50000000000026290, -2.500000000000000000 ) ) ;
#1931 = ORIENTED_EDGE ( 'NONE', *, *, #7024, .F. ) ;
#1932 = SURFACE_SIDE_STYLE ('',( #9148 ) ) ;
#1933 = CIRCLE ( 'NONE', #492, 20.00000000000000355 ) ;
#1934 = CARTESIAN_POINT ( 'NONE',  ( 2.500000000000010214, 28.96446609406726225, 15.76562500000000178 ) ) ;
#1935 = CARTESIAN_POINT ( 'NONE',  ( -25.98076211353311393, 53.43749999808803608, -3.000000000000132339 ) ) ;
#1936 = PRODUCT_RELATED_PRODUCT_CATEGORY ( 'part', '', ( #466 ) ) ;
#1937 = ADVANCED_FACE ( 'NONE', ( #9856 ), #8080, .T. ) ;
#1938 = CARTESIAN_POINT ( 'NONE',  ( -25.44486372867087809, 54.86876073720499392, -3.000000000000132339 ) ) ;
#1939 = LINE ( 'NONE', #254, #798 ) ;
#1940 = EDGE_CURVE ( 'NONE', #7929, #8762, #512, .T. ) ;
#1941 = VECTOR ( 'NONE', #456, 1000.000000000000000 ) ;
#1942 = LINE ( 'NONE', #6205, #9085 ) ;
#1943 = FACE_OUTER_BOUND ( 'NONE', #9037, .T. ) ;
#1944 = VERTEX_POINT ( 'NONE', #3393 ) ;
#1945 =( BOUNDED_CURVE ( )  B_SPLINE_CURVE ( 2, ( #6608, #615, #10729, #3854, #4011, #7397, #1461, #453, #6503 ),
 .UNSPECIFIED., .F., .F. ) 
 B_SPLINE_CURVE_WITH_KNOTS ( ( 3, 2, 2, 2, 3 ),
 ( 0.4166666666666666297, 0.4259259259259259300, 0.4444444444444444198, 0.4629629629629629650, 0.4722222222222222099 ),
 .UNSPECIFIED. ) 
 CURVE ( )  GEOMETRIC_REPRESENTATION_ITEM ( )  RATIONAL_B_SPLINE_CURVE ( ( 0.9330127018922194093, 0.9330127018922191873, 1.000000000000000000, 0.8660254037844387076, 1.000000000000000000, 0.8660254037844387076, 1.000000000000000000, 0.9330127018922194093, 0.9330127018922194093 ) ) 
 REPRESENTATION_ITEM ( '' )  );
#1946 = ORIENTED_EDGE ( 'NONE', *, *, #6985, .T. ) ;
#1947 = CARTESIAN_POINT ( 'NONE',  ( -26.98076211353309972, 54.86666666666653214, -3.267949192431252037 ) ) ;
#1948 = ADVANCED_FACE ( 'NONE', ( #10944 ), #6723, .T. ) ;
#1949 = LINE ( 'NONE', #7154, #8068 ) ;
#1950 =( NAMED_UNIT ( * ) SI_UNIT ( $, .STERADIAN. ) SOLID_ANGLE_UNIT ( ) );
#1951 = VERTEX_POINT ( 'NONE', #1413 ) ;
#1952 = FACE_OUTER_BOUND ( 'NONE', #3781, .T. ) ;
#1953 = PLANE ( 'NONE',  #1870 ) ;
#1954 = ADVANCED_FACE ( 'NONE', ( #4806 ), #826, .T. ) ;
#1955 = CARTESIAN_POINT ( 'NONE',  ( 16.69520167530635746, 18.25454579299907465, 11.16417930307855677 ) ) ;
#1956 = DIRECTION ( 'NONE',  ( 0.000000000000000000, 0.000000000000000000, 1.000000000000000000 ) ) ;
#1957 = CARTESIAN_POINT ( 'NONE',  ( -27.60187600103308014, 52.40208333237728056, -4.064049460664955760 ) ) ;
#1958 = LINE ( 'NONE', #7002, #1646 ) ;
#1959 = VERTEX_POINT ( 'NONE', #7243 ) ;
#1960 = CARTESIAN_POINT ( 'NONE',  ( 29.50000000000000711, 2.000000000000001776, -12.50000000000000000 ) ) ;
#1961 = ORIENTED_EDGE ( 'NONE', *, *, #10826, .F. ) ;
#1962 = CARTESIAN_POINT ( 'NONE',  ( -0.9693646802875608426, 27.47259180932603684, 14.45531658473306535 ) ) ;
#1963 = ORIENTED_EDGE ( 'NONE', *, *, #2382, .F. ) ;
#1964 = CARTESIAN_POINT ( 'NONE',  ( 16.90694777372845437, 16.62861179130368683, 12.08020438729360180 ) ) ;
#1965 = CARTESIAN_POINT ( 'NONE',  ( -25.98076211353311393, 49.49999999999986500, -5.000000000000103029 ) ) ;
#1966 = CARTESIAN_POINT ( 'NONE',  ( 19.95755123817951215, 17.62047157401400810, 12.00579112326941988 ) ) ;
#1967 = CARTESIAN_POINT ( 'NONE',  ( -25.17020516978313083, 53.33541666571061768, -6.403925809002825709 ) ) ;
#1968 = DIRECTION ( 'NONE',  ( 0.000000000000000000, 0.000000000000000000, -1.000000000000000000 ) ) ;
#1969 = FACE_OUTER_BOUND ( 'NONE', #4251, .T. ) ;
#1970 = DIRECTION ( 'NONE',  ( -1.000000000000000000, -0.000000000000000000, -0.000000000000000000 ) ) ;
#1971 = EDGE_LOOP ( 'NONE', ( #9546, #6752, #9684, #9152 ) ) ;
#1972 = EDGE_CURVE ( 'NONE', #2160, #2294, #6718, .T. ) ;
#1973 = FACE_OUTER_BOUND ( 'NONE', #8882, .T. ) ;
#1974 = CARTESIAN_POINT ( 'NONE',  ( -25.98076211353311393, 49.49999999999986500, -3.000000000000131894 ) ) ;
#1975 = DIRECTION ( 'NONE',  ( 1.000000000000000000, 0.000000000000000000, 0.000000000000000000 ) ) ;
#1976 = CARTESIAN_POINT ( 'NONE',  ( -25.98076211353311393, 49.49999999999986500, -7.000000000000074607 ) ) ;
#1977 = DIRECTION ( 'NONE',  ( 0.000000000000000000, 0.000000000000000000, -1.000000000000000000 ) ) ;
#1978 = LINE ( 'NONE', #350, #9543 ) ;
#1979 = CARTESIAN_POINT ( 'NONE',  ( -3.500000000000005329, 30.06616922564516869, 17.46655841526694175 ) ) ;
#1980 = DIRECTION ( 'NONE',  ( 0.000000000000000000, 1.224646799147353207E-16, 1.000000000000000000 ) ) ;
#1981 = ORIENTED_EDGE ( 'NONE', *, *, #5666, .F. ) ;
#1982 = CARTESIAN_POINT ( 'NONE',  ( -25.98076211353324894, 13.49999999999941913, -5.000000000000000000 ) ) ;
#1983 = VECTOR ( 'NONE', #10089, 1000.000000000000000 ) ;
#1984 = CARTESIAN_POINT ( 'NONE',  ( -2.469212770973128190, 29.60886282244813117, 16.49922112211940117 ) ) ;
#1985 = CARTESIAN_POINT ( 'NONE',  ( 1.767766952966377314, 28.23223304703363112, 14.43750000000000178 ) ) ;
#1986 = FACE_OUTER_BOUND ( 'NONE', #10458, .T. ) ;
#1987 = CARTESIAN_POINT ( 'NONE',  ( 0.02993401039713504061, 2.688325911136429713, -2.343682934607792312 ) ) ;
#1988 = AXIS2_PLACEMENT_3D ( 'NONE', #1824, #7049, #6206 ) ;
#1989 = CARTESIAN_POINT ( 'NONE',  ( -26.79131905728310059, 51.06041666571061199, -3.596074190997381237 ) ) ;
#1990 = CARTESIAN_POINT ( 'NONE',  ( 0.000000000000000000, 2.020667218593133248E-16, -1.650000000000000355 ) ) ;
#1991 = CARTESIAN_POINT ( 'NONE',  ( -25.98076211353311393, 55.27499999999986358, -7.309401076758571314 ) ) ;
#1992 = ORIENTED_EDGE ( 'NONE', *, *, #4028, .T. ) ;
#1993 = ORIENTED_EDGE ( 'NONE', *, *, #1324, .T. ) ;
#1994 = CARTESIAN_POINT ( 'NONE',  ( 27.50000000000001066, -8.499999999999984013, 10.00000000000001243 ) ) ;
#1995 = DIRECTION ( 'NONE',  ( 1.000000000000000000, 6.098637220230964906E-17, 0.000000000000000000 ) ) ;
#1996 = ORIENTED_EDGE ( 'NONE', *, *, #6985, .F. ) ;
#1997 = DIRECTION ( 'NONE',  ( 1.000000000000000000, -0.000000000000000000, -0.000000000000000000 ) ) ;
#1998 = CARTESIAN_POINT ( 'NONE',  ( 4.000000000000000000, 2.309401076758497151, -3.433295621305379353 ) ) ;
#1999 = CONICAL_SURFACE ( 'NONE', #3944, 2.041999999999999815, 1.047197551196591858 ) ;
#2000 = CARTESIAN_POINT ( 'NONE',  ( 23.26254143866440671, 20.58647472722595850, 11.00732503135576401 ) ) ;
#2001 = ADVANCED_FACE ( 'NONE', ( #3858, #51 ), #5945, .F. ) ;
#2002 = CARTESIAN_POINT ( 'NONE',  ( -3.500000000000002665, 29.72450764647708255, 16.48359592357600789 ) ) ;
#2003 = EDGE_CURVE ( 'NONE', #4635, #3058, #8504, .T. ) ;
#2004 = CARTESIAN_POINT ( 'NONE',  ( -24.35964822603314772, 53.45208333237727771, -5.935950539335252074 ) ) ;
#2005 = LINE ( 'NONE', #2364, #10865 ) ;
#2006 = B_SPLINE_CURVE_WITH_KNOTS ( 'NONE', 3,
 ( #538, #6588, #490, #2221, #5768, #3938, #7324, #9153 ),
 .UNSPECIFIED., .F., .F.,
 ( 4, 2, 2, 4 ),
 ( 0.000000000000000000, 0.002450665683189818828, 0.003675998524784728459, 0.004901331366379638524 ),
 .UNSPECIFIED. ) ;
#2007 = ORIENTED_EDGE ( 'NONE', *, *, #10625, .F. ) ;
#2008 = CARTESIAN_POINT ( 'NONE',  ( 0.000000000000000000, 0.000000000000000000, 3.499999999999999556 ) ) ;
#2009 = ORIENTED_EDGE ( 'NONE', *, *, #1458, .F. ) ;
#2010 = CARTESIAN_POINT ( 'NONE',  ( -1.814555661125939912, 31.72097824480680117, 14.06469158473306358 ) ) ;
#2011 = ORIENTED_EDGE ( 'NONE', *, *, #1380, .F. ) ;
#2012 = CARTESIAN_POINT ( 'NONE',  ( 15.40853749019034069, 18.12699641572163145, 12.22072830420661660 ) ) ;
#2013 = CARTESIAN_POINT ( 'NONE',  ( 18.86745781575159242, 21.66267592685425569, 11.95042449705185561 ) ) ;
#2014 = CARTESIAN_POINT ( 'NONE',  ( 21.93767140838681584, 18.93041396519599928, 13.00425721518307576 ) ) ;
#2015 = ADVANCED_FACE ( 'NONE', ( #1727 ), #3351, .F. ) ;
#2016 = CARTESIAN_POINT ( 'NONE',  ( -26.79131905728310059, 53.45208333237728482, -6.403925809002825709 ) ) ;
#2017 = LINE ( 'NONE', #1915, #5074 ) ;
#2018 = PLANE ( 'NONE',  #10066 ) ;
#2019 = EDGE_LOOP ( 'NONE', ( #8209, #7298, #5855, #6764 ) ) ;
#2020 = DIRECTION ( 'NONE',  ( 0.000000000000000000, 0.000000000000000000, 1.000000000000000000 ) ) ;
#2021 = PLANE ( 'NONE',  #1000 ) ;
#2022 = CARTESIAN_POINT ( 'NONE',  ( -21.65063509461104374, 12.49999999999986322, -2.500000000000000000 ) ) ;
#2023 = LINE ( 'NONE', #9746, #1702 ) ;
#2024 = CARTESIAN_POINT ( 'NONE',  ( -26.98076211353309972, 55.94583333142136894, -6.732050807568954909 ) ) ;
#2025 = CARTESIAN_POINT ( 'NONE',  ( -26.98076211353309972, 52.67916666475470322, -3.267949192431252037 ) ) ;
#2026 = CARTESIAN_POINT ( 'NONE',  ( 0.000000000000000000, 0.000000000000000000, -2.500000000000000000 ) ) ;
#2027 = CARTESIAN_POINT ( 'NONE',  ( 0.000000000000000000, 2.357898499370433054, -1.951563910473907981E-15 ) ) ;
#2028 = CARTESIAN_POINT ( 'NONE',  ( 3.500000000000005773, 31.44974746830583356, 14.67187500000000178 ) ) ;
#2029 = CARTESIAN_POINT ( 'NONE',  ( -0.3461262719736137305, 4.658553426539289610, -3.671615880910373608 ) ) ;
#2030 = CIRCLE ( 'NONE', #10190, 5.000000000000000888 ) ;
#2031 = EDGE_CURVE ( 'NONE', #9170, #10481, #7798, .T. ) ;
#2032 = ORIENTED_EDGE ( 'NONE', *, *, #1115, .F. ) ;
#2033 = CARTESIAN_POINT ( 'NONE',  ( 34.99999999999987210, 2.000000000000002220, 17.49999999999999645 ) ) ;
#2034 = CARTESIAN_POINT ( 'NONE',  ( 1.767766952966372429, 31.76776695296637598, 16.00000000000000355 ) ) ;
#2035 = CARTESIAN_POINT ( 'NONE',  ( 4.207491450040567571, -2.029819825146485179, -3.671670828759567407 ) ) ;
#2036 = VECTOR ( 'NONE', #630, 1000.000000000000000 ) ;
#2037 = CARTESIAN_POINT ( 'NONE',  ( 21.51635413324704160, 18.70478684647606826, 12.00579112326941988 ) ) ;
#2038 = CARTESIAN_POINT ( 'NONE',  ( 29.49999999999999289, -7.999999999999996447, 17.50000000000000000 ) ) ;
#2039 = CARTESIAN_POINT ( 'NONE',  ( -4.000000000000000000, -0.3979232138631226823, -3.896351557369779711E-17 ) ) ;
#2040 = CARTESIAN_POINT ( 'NONE',  ( -2.807080416178626692, 3.225969019225154444, -3.502507215260441065 ) ) ;
#2041 = CARTESIAN_POINT ( 'NONE',  ( -25.17020516978313083, 51.87708333237728198, -3.596074190997380349 ) ) ;
#2042 = DIRECTION ( 'NONE',  ( -0.5000000000000061062, 1.060575238724902601E-16, -0.8660254037844351549 ) ) ;
#2043 = CARTESIAN_POINT ( 'NONE',  ( -25.98076211353311393, 54.22499999999986642, -2.690598923241634743 ) ) ;
#2044 = CIRCLE ( 'NONE', #5244, 4.999999999999997335 ) ;
#2045 = ORIENTED_EDGE ( 'NONE', *, *, #4707, .F. ) ;
#2046 = VECTOR ( 'NONE', #6825, 1000.000000000000000 ) ;
#2047 = VERTEX_POINT ( 'NONE', #4641 ) ;
#2048 = DIRECTION ( 'NONE',  ( 0.000000000000000000, 0.000000000000000000, 1.000000000000000000 ) ) ;
#2049 = CARTESIAN_POINT ( 'NONE',  ( 34.94281041931228771, 2.000000000000002220, -5.500000000000000000 ) ) ;
#2050 = CONTEXT_DEPENDENT_SHAPE_REPRESENTATION ( #1320, #4410 ) ;
#2051 = ORIENTED_EDGE ( 'NONE', *, *, #3763, .F. ) ;
#2052 = DIRECTION ( 'NONE',  ( 1.000000000000000000, 0.000000000000000000, 0.000000000000000000 ) ) ;
#2053 = VECTOR ( 'NONE', #9065, 1000.000000000000000 ) ;
#2054 = CARTESIAN_POINT ( 'NONE',  ( -27.60187600103308725, 50.71041666571061768, -5.935950539335252074 ) ) ;
#2055 = CIRCLE ( 'NONE', #7923, 3.369999999999997886 ) ;
#2056 = EDGE_CURVE ( 'NONE', #3381, #7103, #2651, .T. ) ;
#2057 = CARTESIAN_POINT ( 'NONE',  ( 19.42818427286271898, 22.60367925258928068, 10.95195840513898489 ) ) ;
#2058 = ORIENTED_EDGE ( 'NONE', *, *, #10990, .F. ) ;
#2059 = CARTESIAN_POINT ( 'NONE',  ( -25.17020516978313083, 52.11041666571060915, -6.403925809002825709 ) ) ;
#2060 = AXIS2_PLACEMENT_3D ( 'NONE', #4354, #9346, #1678 ) ;
#2061 = VERTEX_POINT ( 'NONE', #8182 ) ;
#2062 = LINE ( 'NONE', #7164, #5810 ) ;
#2063 = ORIENTED_EDGE ( 'NONE', *, *, #10758, .T. ) ;
#2064 = CARTESIAN_POINT ( 'NONE',  ( -2.458860273309268152, 29.54350846364475203, 15.50141270685246830 ) ) ;
#2065 = TOROIDAL_SURFACE ( 'NONE', #1525, 4.000000000000000000, 0.2500000000000000000 ) ;
#2066 = ORIENTED_EDGE ( 'NONE', *, *, #3077, .F. ) ;
#2067 = CARTESIAN_POINT ( 'NONE',  ( 18.88912242859132107, 19.99746927611068870, 11.95042449705224819 ) ) ;
#2068 = EDGE_CURVE ( 'NONE', #947, #10875, #5453, .T. ) ;
#2069 = DIRECTION ( 'NONE',  ( 0.000000000000000000, 0.000000000000000000, -1.000000000000000000 ) ) ;
#2070 = ADVANCED_FACE ( 'NONE', ( #4696 ), #6294, .T. ) ;
#2071 = CARTESIAN_POINT ( 'NONE',  ( 22.92515349615029407, 19.68371071013345741, 13.00425721518307753 ) ) ;
#2073 = CARTESIAN_POINT ( 'NONE',  ( -27.60187600103308014, 54.91041666571061342, -5.935950539335252074 ) ) ;
#2072 = AXIS2_PLACEMENT_3D ( 'NONE', #9436, #3758, #4652 ) ;
#2074 = FACE_OUTER_BOUND ( 'NONE', #8763, .T. ) ;
#2075 = CARTESIAN_POINT ( 'NONE',  ( -23.98076211353314235, 50.11249999808803324, -5.000000000000103029 ) ) ;
#2076 = CARTESIAN_POINT ( 'NONE',  ( 2.649999999999991029, 30.00000000000000000, -2.500000000000000000 ) ) ;
#2077 = ORIENTED_EDGE ( 'NONE', *, *, #6021, .F. ) ;
#2078 = EDGE_LOOP ( 'NONE', ( #904, #5617, #328, #7180 ) ) ;
#2079 = CARTESIAN_POINT ( 'NONE',  ( 19.38642580597931087, 17.15576104669793267, 13.00425794126423362 ) ) ;
#2080 = EDGE_CURVE ( 'NONE', #7845, #9793, #4, .T. ) ;
#2081 = CARTESIAN_POINT ( 'NONE',  ( 2.500000000000000000, 2.357898499370433054, -1.951563910473907981E-15 ) ) ;
#2082 = CARTESIAN_POINT ( 'NONE',  ( -23.98076211353314235, 50.25833333333320496, -6.154700538379337615 ) ) ;
#2083 = LINE ( 'NONE', #9524, #8086 ) ;
#2084 = CARTESIAN_POINT ( 'NONE',  ( -25.98076211353311393, 53.87499999999986500, -7.000000000000072831 ) ) ;
#2085 = LINE ( 'NONE', #1301, #5488 ) ;
#2086 = CARTESIAN_POINT ( 'NONE',  ( 3.061158938895378157, 2.351840044243081795, 2.926493552096017137 ) ) ;
#2087 = CARTESIAN_POINT ( 'NONE',  ( 29.17190429162963738, 6.999999999999999112, -2.500000000000000000 ) ) ;
#2088 = EDGE_CURVE ( 'NONE', #1662, #10997, #5832, .T. ) ;
#2089 = EDGE_CURVE ( 'NONE', #2779, #3903, #2085, .T. ) ;
#2090 = PLANE ( 'NONE',  #3345 ) ;
#2091 = CARTESIAN_POINT ( 'NONE',  ( -1.449747468305836229, 33.50000000000000000, 14.98437500000000711 ) ) ;
#2092 = DIRECTION ( 'NONE',  ( -1.000000000000000000, -0.000000000000000000, -0.000000000000000000 ) ) ;
#2093 = ORIENTED_EDGE ( 'NONE', *, *, #9306, .F. ) ;
#2094 = CARTESIAN_POINT ( 'NONE',  ( 1.449747468305833120, 33.50000000000000000, 14.82812500000000178 ) ) ;
#2095 = AXIS2_PLACEMENT_3D ( 'NONE', #2695, #7635, #1916 ) ;
#2096 = AXIS2_PLACEMENT_3D ( 'NONE', #1965, #5299, #8685 ) ;
#2097 = CARTESIAN_POINT ( 'NONE',  ( -1.035533905932742638, 32.50000000000000000, 16.23437500000000355 ) ) ;
#2098 = PLANE ( 'NONE',  #3491 ) ;
#2099 = CARTESIAN_POINT ( 'NONE',  ( -27.60187600103308370, 55.84374999904394343, -5.000000000000103029 ) ) ;
#2100 = CARTESIAN_POINT ( 'NONE',  ( -24.98076211353312814, 53.11666666666652503, -6.732050807568954909 ) ) ;
#2101 = CARTESIAN_POINT ( 'NONE',  ( -3.522875095019672109, 2.820352903225427532, -3.598441714920591394 ) ) ;
#2102 = CARTESIAN_POINT ( 'NONE',  ( -26.79131905728310059, 51.52708333237728056, -6.403925809002825709 ) ) ;
#2103 = PRODUCT_DEFINITION_SHAPE ( 'NONE', 'NONE',  #1375 ) ;
#2104 = DIRECTION ( 'NONE',  ( -1.156482317317871725E-16, 2.312964634635742464E-16, 1.000000000000000000 ) ) ;
#2105 = MECHANICAL_DESIGN_GEOMETRIC_PRESENTATION_REPRESENTATION (  '', ( #6704 ), #8842 ) ;
#2106 = DIRECTION ( 'NONE',  ( 0.000000000000000000, 0.000000000000000000, 1.000000000000000000 ) ) ;
#2107 = ORIENTED_EDGE ( 'NONE', *, *, #6968, .F. ) ;
#2108 = CONICAL_SURFACE ( 'NONE', #1031, 4.624785217660733139, 1.047197551196604071 ) ;
#2109 = DIRECTION ( 'NONE',  ( 0.000000000000000000, 0.000000000000000000, -1.000000000000000000 ) ) ;
#2110 = EDGE_CURVE ( 'NONE', #2436, #9774, #4753, .T. ) ;
#2111 = CARTESIAN_POINT ( 'NONE',  ( -2.500000000000000444, 3.061616997868383634E-16, -5.000000000000000888 ) ) ;
#2112 = SHAPE_DEFINITION_REPRESENTATION ( #2630, #10603 ) ;
#2113 = EDGE_LOOP ( 'NONE', ( #6669, #9050, #7283, #4140 ) ) ;
#2114 = VECTOR ( 'NONE', #6232, 1000.000000000000000 ) ;
#2115 = DIRECTION ( 'NONE',  ( -0.000000000000000000, 1.000000000000000000, -0.000000000000000000 ) ) ;
#2116 = CARTESIAN_POINT ( 'NONE',  ( 25.71106610644839208, 0.000000000000000000, 14.50000000000000000 ) ) ;
#2117 = AXIS2_PLACEMENT_3D ( 'NONE', #8865, #1247, #510 ) ;
#2118 = CARTESIAN_POINT ( 'NONE',  ( 22.83430298279833437, 18.47273307877622983, 10.95195840513859231 ) ) ;
#2119 = ORIENTED_EDGE ( 'NONE', *, *, #8304, .T. ) ;
#2120 = CARTESIAN_POINT ( 'NONE',  ( -24.35964822603314417, 51.29374999904394627, -5.000000000000103029 ) ) ;
#2121 = EDGE_LOOP ( 'NONE', ( #4568, #2616, #10712, #10894 ) ) ;
#2122 = LINE ( 'NONE', #7898, #9725 ) ;
#2123 = ORIENTED_EDGE ( 'NONE', *, *, #242, .T. ) ;
#2124 = CARTESIAN_POINT ( 'NONE',  ( 2.500000000000007550, 31.03553390593274486, 14.67187500000000178 ) ) ;
#2125 = SURFACE_SIDE_STYLE ('',( #4736 ) ) ;
#2126 = ORIENTED_EDGE ( 'NONE', *, *, #6854, .T. ) ;
#2127 = EDGE_CURVE ( 'NONE', #8043, #3326, #7249, .T. ) ;
#2128 = CARTESIAN_POINT ( 'NONE',  ( 23.59820535295391508, 19.10314065948846718, 10.95195840513859231 ) ) ;
#2129 = CARTESIAN_POINT ( 'NONE',  ( -4.024497503033519941, -2.323544716729390558, -3.572167766733381544 ) ) ;
#2130 = CARTESIAN_POINT ( 'NONE',  ( 19.58285320134683261, 17.29236643726018130, 13.00425622583864715 ) ) ;
#2131 = CARTESIAN_POINT ( 'NONE',  ( 2.500000000000000000, -1.768423874527823791, -1.020999999999998353 ) ) ;
#2132 = DIRECTION ( 'NONE',  ( 0.000000000000000000, 0.000000000000000000, 1.000000000000000000 ) ) ;
#2133 = ORIENTED_EDGE ( 'NONE', *, *, #2996, .T. ) ;
#2134 = VERTEX_POINT ( 'NONE', #10528 ) ;
#2135 = CARTESIAN_POINT ( 'NONE',  ( 16.16243297953557700, 18.78731448874862053, 13.21853671947355302 ) ) ;
#2136 = CARTESIAN_POINT ( 'NONE',  ( 27.50000000000000711, 0.5000000000000162093, 10.00000000000000888 ) ) ;
#2137 = CARTESIAN_POINT ( 'NONE',  ( -25.98076211353311393, 59.49999999999985789, -7.000000000000074607 ) ) ;
#2138 = DIRECTION ( 'NONE',  ( -1.000000000000000000, -6.098637220230963674E-17, -0.000000000000000000 ) ) ;
#2139 = DIRECTION ( 'NONE',  ( 1.000000000000000000, 0.000000000000000000, 0.000000000000000000 ) ) ;
#2140 = DIRECTION ( 'NONE',  ( 0.000000000000000000, 0.000000000000000000, -1.000000000000000000 ) ) ;
#2141 = DIRECTION ( 'NONE',  ( 1.000000000000000000, -0.000000000000000000, 1.156482317317871478E-16 ) ) ;
#2142 = CARTESIAN_POINT ( 'NONE',  ( -3.500000000000003109, 29.99999999999999645, 15.21875000000000355 ) ) ;
#2143 = DIRECTION ( 'NONE',  ( 0.000000000000000000, 0.000000000000000000, 1.000000000000000000 ) ) ;
#2144 = EDGE_CURVE ( 'NONE', #7845, #3061, #8754, .T. ) ;
#2145 = ORIENTED_EDGE ( 'NONE', *, *, #6147, .T. ) ;
#2146 = FILL_AREA_STYLE ('',( #5824 ) ) ;
#2147 = EDGE_CURVE ( 'NONE', #7593, #609, #6240, .T. ) ;
#2148 = CARTESIAN_POINT ( 'NONE',  ( -3.467250377026234176, 29.51776231023078623, 17.49702953738633937 ) ) ;
#2149 = CARTESIAN_POINT ( 'NONE',  ( 0.06616922564517314920, 33.50000000000000000, 14.65405841526694353 ) ) ;
#2150 = CARTESIAN_POINT ( 'NONE',  ( 0.000000000000000000, 0.000000000000000000, 2.500000000000000000 ) ) ;
#2151 = CARTESIAN_POINT ( 'NONE',  ( -27.44132740410865523, 55.89336612041927310, -4.296608737464627126 ) ) ;
#2152 = CARTESIAN_POINT ( 'NONE',  ( -23.98076211353314235, 53.61249999808804034, -5.000000000000103029 ) ) ;
#2153 = CARTESIAN_POINT ( 'NONE',  ( -26.79131905728310059, 53.16041666571061342, -3.596074190997381237 ) ) ;
#2154 = FACE_OUTER_BOUND ( 'NONE', #9138, .T. ) ;
#2155 = PLANE ( 'NONE',  #94 ) ;
#2156 = VECTOR ( 'NONE', #5024, 1000.000000000000000 ) ;
#2157 = ORIENTED_EDGE ( 'NONE', *, *, #3221, .F. ) ;
#2158 = FACE_OUTER_BOUND ( 'NONE', #10771, .T. ) ;
#2159 = ITEM_DEFINED_TRANSFORMATION ( 'NONE', 'NONE', #9350,  #308 ) ;
#2160 = VERTEX_POINT ( 'NONE', #3746 ) ;
#2161 = CARTESIAN_POINT ( 'NONE',  ( 2.500000000000000000, 1.178949249685213863, -2.042000000000001148 ) ) ;
#2162 = CIRCLE ( 'NONE', #8360, 2.100000000000000089 ) ;
#2163 = CARTESIAN_POINT ( 'NONE',  ( -26.79131905728310059, 50.18541666571061199, -3.596074190997381237 ) ) ;
#2164 = CARTESIAN_POINT ( 'NONE',  ( 17.31910053175343478, 17.63064693655086757, 11.10566822806672427 ) ) ;
#2165 = ORIENTED_EDGE ( 'NONE', *, *, #2068, .T. ) ;
#2166 = DIRECTION ( 'NONE',  ( 0.000000000000000000, 0.000000000000000000, 1.000000000000000000 ) ) ;
#2168 = ORIENTED_EDGE ( 'NONE', *, *, #6266, .F. ) ;
#2167 = EDGE_CURVE ( 'NONE', #7719, #4463, #2464, .T. ) ;
#2169 = DIRECTION ( 'NONE',  ( 1.000000000000000000, 0.000000000000000000, 0.000000000000000000 ) ) ;
#2170 = ORIENTED_EDGE ( 'NONE', *, *, #9755, .F. ) ;
#2171 = CARTESIAN_POINT ( 'NONE',  ( -2.500000000000005773, 29.99999999999999645, 13.96875000000000355 ) ) ;
#2172 = ORIENTED_EDGE ( 'NONE', *, *, #1783, .F. ) ;
#2173 = CARTESIAN_POINT ( 'NONE',  ( 22.95140240311772573, 18.55416269319264444, 10.95195840513845553 ) ) ;
#2174 = CIRCLE ( 'NONE', #9259, 2.000000000000000000 ) ;
#2175 = CARTESIAN_POINT ( 'NONE',  ( 4.024499207728657879, 2.323545700935571556, -3.572172305156506411 ) ) ;
#2176 = CARTESIAN_POINT ( 'NONE',  ( 21.54797068462080745, 18.65933514708097007, 13.00425721518307576 ) ) ;
#2177 = CARTESIAN_POINT ( 'NONE',  ( -27.98076211353308551, 52.56249999808803608, -5.000000000000103029 ) ) ;
#2178 = AXIS2_PLACEMENT_3D ( 'NONE', #9556, #8722, #1956 ) ;
#2179 = CARTESIAN_POINT ( 'NONE',  ( 34.91794119163850496, 2.397787035234373310, -3.994322637888108485 ) ) ;
#2180 = CARTESIAN_POINT ( 'NONE',  ( -26.11323168687438212, 59.00000000000083134, -7.000000000000075495 ) ) ;
#2181 = ORIENTED_EDGE ( 'NONE', *, *, #2382, .T. ) ;
#2182 = ORIENTED_EDGE ( 'NONE', *, *, #6710, .F. ) ;
#2183 = CARTESIAN_POINT ( 'NONE',  ( 18.83452698454826901, 16.95224361855724737, 13.01423506301239819 ) ) ;
#2184 = DIRECTION ( 'NONE',  ( -1.000000000000000000, -6.098637220230963674E-17, -1.156482317317871478E-16 ) ) ;
#2185 = CARTESIAN_POINT ( 'NONE',  ( -27.98076211353308551, 49.90833333333318933, -3.845299461620869330 ) ) ;
#2186 = DIRECTION ( 'NONE',  ( 0.000000000000000000, 0.000000000000000000, -1.000000000000000000 ) ) ;
#2187 = DIRECTION ( 'NONE',  ( -1.000000000000000000, -0.000000000000000000, -0.000000000000000000 ) ) ;
#2188 = CARTESIAN_POINT ( 'NONE',  ( -3.500000000000003553, 31.44974746830583356, 13.89062500000000355 ) ) ;
#2189 = DIRECTION ( 'NONE',  ( 0.000000000000000000, -1.000000000000000000, 0.000000000000000000 ) ) ;
#2190 = UNCERTAINTY_MEASURE_WITH_UNIT (LENGTH_MEASURE( 1.000000000000000082E-05 ), #401, 'distance_accuracy_value', 'NONE');
#2191 = ORIENTED_EDGE ( 'NONE', *, *, #9063, .F. ) ;
#2192 = DIRECTION ( 'NONE',  ( 1.000000000000000000, 6.098637220230963674E-17, -0.000000000000000000 ) ) ;
#2193 = CARTESIAN_POINT ( 'NONE',  ( 1.720978244806812496, 28.18544433887406342, 16.68530841526694175 ) ) ;
#2194 = DIRECTION ( 'NONE',  ( -0.000000000000000000, -1.000000000000000000, -0.000000000000000000 ) ) ;
#2195 = CARTESIAN_POINT ( 'NONE',  ( 0.000000000000000000, 0.000000000000000000, 0.000000000000000000 ) ) ;
#2196 = CARTESIAN_POINT ( 'NONE',  ( 29.50000000000000711, 2.000000000000001776, 5.500000000000001776 ) ) ;
#2197 = EDGE_CURVE ( 'NONE', #5599, #9687, #5106, .T. ) ;
#2198 = CARTESIAN_POINT ( 'NONE',  ( 0.000000000000000000, -3.031088913245550298, -1.749999999999972911 ) ) ;
#2199 = CARTESIAN_POINT ( 'NONE',  ( -27.60187600103308370, 53.04374999904394627, -5.000000000000103029 ) ) ;
#2200 = VECTOR ( 'NONE', #6936, 1000.000000000000000 ) ;
#2201 = EDGE_CURVE ( 'NONE', #9227, #3885, #4970, .T. ) ;
#2202 = CARTESIAN_POINT ( 'NONE',  ( 1.654252653721905331, 3.663718938583014229, -0.01223254789873410957 ) ) ;
#2203 = DIRECTION ( 'NONE',  ( -1.000000000000000000, -6.098637220230964906E-17, 0.000000000000000000 ) ) ;
#2204 = ORIENTED_EDGE ( 'NONE', *, *, #6466, .T. ) ;
#2205 = CARTESIAN_POINT ( 'NONE',  ( -23.98076211353314235, 54.25416666475469185, -3.845299461620867554 ) ) ;
#2206 = PLANE ( 'NONE',  #2741 ) ;
#2207 = CONTEXT_DEPENDENT_SHAPE_REPRESENTATION ( #6276, #5472 ) ;
#2208 = ORIENTED_EDGE ( 'NONE', *, *, #6301, .T. ) ;
#2209 = CIRCLE ( 'NONE', #1498, 5.384454397937118664 ) ;
#2210 = CARTESIAN_POINT ( 'NONE',  ( -24.35964822603314417, 51.99374999904394201, -5.000000000000103029 ) ) ;
#2211 = ADVANCED_FACE ( 'NONE', ( #10845 ), #8343, .F. ) ;
#2212 = CARTESIAN_POINT ( 'NONE',  ( -27.60187600103308370, 50.76874999904395480, -5.000000000000103029 ) ) ;
#2213 = AXIS2_PLACEMENT_3D ( 'NONE', #5591, #4709, #8244 ) ;
#2214 = CLOSED_SHELL ( 'NONE', ( #1051, #3862, #5210, #5185, #7508, #1194, #1689, #4401 ) ) ;
#2215 = CARTESIAN_POINT ( 'NONE',  ( 17.36588923991300604, 17.58385822839129986, 12.10347664333366247 ) ) ;
#2216 = VECTOR ( 'NONE', #1431, 1000.000000000000000 ) ;
#2217 = ORIENTED_EDGE ( 'NONE', *, *, #158, .F. ) ;
#2218 = EDGE_CURVE ( 'NONE', #5054, #1254, #6733, .T. ) ;
#2219 = CARTESIAN_POINT ( 'NONE',  ( -25.98076211353311393, 53.78749999808803040, -7.000000000000072831 ) ) ;
#2220 = ORIENTED_EDGE ( 'NONE', *, *, #3035, .F. ) ;
#2221 = CARTESIAN_POINT ( 'NONE',  ( -2.449848172108560540, -3.432307619358754724, -3.503702292528910078 ) ) ;
#2222 = VERTEX_POINT ( 'NONE', #5788 ) ;
#2223 = CARTESIAN_POINT ( 'NONE',  ( -2.500000000000004441, 28.96446609406725159, 15.29687500000000178 ) ) ;
#2224 = PRESENTATION_STYLE_ASSIGNMENT (( #4679 ) ) ;
#2225 = ORIENTED_EDGE ( 'NONE', *, *, #8168, .F. ) ;
#2226 = AXIS2_PLACEMENT_3D ( 'NONE', #2807, #8064, #5464 ) ;
#2227 = CARTESIAN_POINT ( 'NONE',  ( 19.12295744889739879, 19.47009535162641569, 11.95042449705107224 ) ) ;
#2228 = AXIS2_PLACEMENT_3D ( 'NONE', #7641, #3363, #9240 ) ;
#2229 = AXIS2_PLACEMENT_3D ( 'NONE', #7271, #10770, #6543 ) ;
#2230 = EDGE_CURVE ( 'NONE', #5764, #10877, #10126, .T. ) ;
#2231 = CARTESIAN_POINT ( 'NONE',  ( 24.49999999999999289, -3.999999999999986233, -4.999999999999992006 ) ) ;
#2232 = CARTESIAN_POINT ( 'NONE',  ( 18.83452698454826901, 16.95224361855724737, 13.01423506301239819 ) ) ;
#2233 = AXIS2_PLACEMENT_3D ( 'NONE', #521, #4927, #5650 ) ;
#2234 = CARTESIAN_POINT ( 'NONE',  ( -25.98076211353311393, 52.38749999808803182, -7.309401076758571314 ) ) ;
#2235 = AXIS2_PLACEMENT_3D ( 'NONE', #3485, #10364, #1980 ) ;
#2236 = CARTESIAN_POINT ( 'NONE',  ( 34.94281041931228771, 2.000000000000002220, 5.500000000000000000 ) ) ;
#2237 = DIRECTION ( 'NONE',  ( 0.000000000000000000, 1.000000000000000000, 0.000000000000000000 ) ) ;
#2238 = ORIENTED_EDGE ( 'NONE', *, *, #8447, .F. ) ;
#2239 = VERTEX_POINT ( 'NONE', #1628 ) ;
#2240 = CARTESIAN_POINT ( 'NONE',  ( 22.11805565807571128, 22.55986279155152374, 12.00579112326941988 ) ) ;
#2241 = AXIS2_PLACEMENT_3D ( 'NONE', #7633, #6509, #2300 ) ;
#2242 = DIRECTION ( 'NONE',  ( 0.000000000000000000, 0.000000000000000000, 1.000000000000000000 ) ) ;
#2243 = DIRECTION ( 'NONE',  ( 0.000000000000000000, 0.000000000000000000, -1.000000000000000000 ) ) ;
#2244 = DIRECTION ( 'NONE',  ( 0.000000000000000000, 1.000000000000000000, 0.000000000000000000 ) ) ;
#2245 = CARTESIAN_POINT ( 'NONE',  ( 0.000000000000000000, 1.178949249685213863, -2.042000000000001148 ) ) ;
#2246 = CARTESIAN_POINT ( 'NONE',  ( -3.500000000000001332, 29.93383077435482065, 14.22094158473306535 ) ) ;
#2247 = DIRECTION ( 'NONE',  ( -1.000000000000000000, -0.000000000000000000, -0.000000000000000000 ) ) ;
#2248 = CARTESIAN_POINT ( 'NONE',  ( 1.411581201560190495E-15, 4.862606272033091592, -3.745885042887436622 ) ) ;
#2249 = DIRECTION ( 'NONE',  ( -1.000000000000000000, 0.000000000000000000, 0.000000000000000000 ) ) ;
#2250 = EDGE_LOOP ( 'NONE', ( #9722, #6708, #2722, #208, #9563, #2628, #427, #9652, #10160, #1123, #3401, #7607, #9046, #2783, #2836 ) ) ;
#2251 = AXIS2_PLACEMENT_3D ( 'NONE', #10250, #4308, #6026 ) ;
#2252 = CARTESIAN_POINT ( 'NONE',  ( -1.720978244806810498, 31.81455566112594013, 16.06030841526693820 ) ) ;
#2253 = CARTESIAN_POINT ( 'NONE',  ( 29.49999999999999289, -3.999999999999993339, 10.00000000000000533 ) ) ;
#2254 = EDGE_CURVE ( 'NONE', #3863, #10456, #6609, .T. ) ;
#2255 = CARTESIAN_POINT ( 'NONE',  ( 16.74199038347050816, 18.20775708483493460, 12.16198771834506509 ) ) ;
#2256 = CARTESIAN_POINT ( 'NONE',  ( -2.500000000000004441, 28.96446609406725514, 14.04687500000000355 ) ) ;
#2257 = CARTESIAN_POINT ( 'NONE',  ( -23.98076211353314235, 51.59999999999985931, -5.000000000000103029 ) ) ;
#2258 = CARTESIAN_POINT ( 'NONE',  ( -27.60187600103308370, 51.46874999904395054, -5.000000000000103029 ) ) ;
#2259 = LINE ( 'NONE', #3873, #10333 ) ;
#2260 = CARTESIAN_POINT ( 'NONE',  ( -0.5449313310646672903, -4.304185902836978883, -3.316620875263469159 ) ) ;
#2261 = VERTEX_POINT ( 'NONE', #776 ) ;
#2262 = AXIS2_PLACEMENT_3D ( 'NONE', #9122, #728, #8293 ) ;
#2263 = VECTOR ( 'NONE', #8699, 1000.000000000000114 ) ;
#2264 = DIRECTION ( 'NONE',  ( 0.000000000000000000, 0.000000000000000000, -1.000000000000000000 ) ) ;
#2265 = CARTESIAN_POINT ( 'NONE',  ( -1.828356344711647319, -3.563200125723192002, -1.076197711133951296E-14 ) ) ;
#2266 = ADVANCED_FACE ( 'NONE', ( #6506 ), #7571, .T. ) ;
#2267 = CONTEXT_DEPENDENT_SHAPE_REPRESENTATION ( #4340, #10436 ) ;
#2268 = EDGE_CURVE ( 'NONE', #3729, #6185, #1081, .T. ) ;
#2269 = DIRECTION ( 'NONE',  ( 0.000000000000000000, 0.000000000000000000, 1.000000000000000000 ) ) ;
#2270 = CARTESIAN_POINT ( 'NONE',  ( -25.98076211353310683, 54.44374999904394485, -3.128098921329806714 ) ) ;
#2271 = AXIS2_PLACEMENT_3D ( 'NONE', #8903, #3738, #2132 ) ;
#2272 = CARTESIAN_POINT ( 'NONE',  ( 21.07346791105437589, 22.52558620363005915, 11.00732503135576401 ) ) ;
#2273 = CARTESIAN_POINT ( 'NONE',  ( -25.17020516978313083, 54.03541666571061342, -6.403925809002825709 ) ) ;
#2274 = ORIENTED_EDGE ( 'NONE', *, *, #6710, .T. ) ;
#2275 = CARTESIAN_POINT ( 'NONE',  ( 34.92403196580097813, 2.306010598194980332, 4.165547504151214220 ) ) ;
#2276 = EDGE_CURVE ( 'NONE', #7380, #7929, #9174, .T. ) ;
#2277 = ORIENTED_EDGE ( 'NONE', *, *, #1271, .F. ) ;
#2278 = FACE_BOUND ( 'NONE', #9260, .T. ) ;
#2280 = VERTEX_POINT ( 'NONE', #3294 ) ;
#2279 = EDGE_CURVE ( 'NONE', #6762, #2549, #5527, .T. ) ;
#2281 = MECHANICAL_DESIGN_GEOMETRIC_PRESENTATION_REPRESENTATION (  '', ( #9019 ), #3880 ) ;
#2282 =( GEOMETRIC_REPRESENTATION_CONTEXT ( 3 ) GLOBAL_UNCERTAINTY_ASSIGNED_CONTEXT ( ( #7877 ) ) GLOBAL_UNIT_ASSIGNED_CONTEXT ( ( #7329, #894, #9891 ) ) REPRESENTATION_CONTEXT ( 'NONE', 'WORKASPACE' ) );
#2283 = LINE ( 'NONE', #2440, #78 ) ;
#2284 = ORIENTED_EDGE ( 'NONE', *, *, #129, .T. ) ;
#2285 = CIRCLE ( 'NONE', #5820, 4.500000000000000000 ) ;
#2286 = CARTESIAN_POINT ( 'NONE',  ( 20.62599888145302529, 16.93661977612163128, 10.95195840513859231 ) ) ;
#2287 = CARTESIAN_POINT ( 'NONE',  ( 0.5276280594147412240, -4.314175951381924889, -3.320322319201654881 ) ) ;
#2288 = CARTESIAN_POINT ( 'NONE',  ( 22.99351140629659795, 23.33806509665494389, 12.94889058896590583 ) ) ;
#2289 = CARTESIAN_POINT ( 'NONE',  ( -27.98076211353308551, 50.40416666475469754, -6.154700538379338504 ) ) ;
#2290 = CARTESIAN_POINT ( 'NONE',  ( 4.000000000000000000, -1.560351142792952617, -0.2242961665059816367 ) ) ;
#2291 = CARTESIAN_POINT ( 'NONE',  ( -27.98076211353308551, 51.22083333142136752, -3.845299461620869330 ) ) ;
#2292 = VERTEX_POINT ( 'NONE', #1679 ) ;
#2293 =( BOUNDED_CURVE ( )  B_SPLINE_CURVE ( 2, ( #1350, #2808, #5408, #7177, #2972, #6346, #7966, #341, #7023 ),
 .UNSPECIFIED., .F., .T. ) 
 B_SPLINE_CURVE_WITH_KNOTS ( ( 3, 2, 2, 2, 3 ),
 ( 0.4166666666666666852, 0.4259259259259259300, 0.4444444444444444198, 0.4629629629629629650, 0.4722222222222222099 ),
 .UNSPECIFIED. ) 
 CURVE ( )  GEOMETRIC_REPRESENTATION_ITEM ( )  RATIONAL_B_SPLINE_CURVE ( ( 0.9330127018922194093, 0.9330127018922195203, 1.000000000000000000, 0.8660254037844387076, 1.000000000000000000, 0.8660254037844387076, 1.000000000000000000, 0.9330127018922194093, 0.9330127018922194093 ) ) 
 REPRESENTATION_ITEM ( '' )  );
#2294 = VERTEX_POINT ( 'NONE', #675 ) ;
#2295 = CARTESIAN_POINT ( 'NONE',  ( 19.72936730704260810, 17.39430066254168139, 13.00425721518307576 ) ) ;
#2296 = DIRECTION ( 'NONE',  ( -1.000000000000000000, 0.000000000000000000, -0.000000000000000000 ) ) ;
#2297 = CARTESIAN_POINT ( 'NONE',  ( 24.49999999999999289, -8.499999999999985789, -4.999999999999992006 ) ) ;
#2298 = LINE ( 'NONE', #8228, #3052 ) ;
#2299 = CARTESIAN_POINT ( 'NONE',  ( -0.06616922564517661864, 33.50000000000000000, 13.90844158473306713 ) ) ;
#2300 = DIRECTION ( 'NONE',  ( 0.000000000000000000, 0.000000000000000000, -1.000000000000000000 ) ) ;
#2301 = LINE ( 'NONE', #7460, #8418 ) ;
#2302 = DIRECTION ( 'NONE',  ( 0.000000000000000000, 0.000000000000000000, 1.000000000000000000 ) ) ;
#2303 = ORIENTED_EDGE ( 'NONE', *, *, #1059, .T. ) ;
#2304 = CARTESIAN_POINT ( 'NONE',  ( 1.814555661125939467, 31.72097824480680828, 15.74780841526694175 ) ) ;
#2305 = FACE_OUTER_BOUND ( 'NONE', #8005, .T. ) ;
#2306 = DIRECTION ( 'NONE',  ( 1.000000000000000000, 6.098637220230963674E-17, 1.156482317317871478E-16 ) ) ;
#2307 = APPLICATION_CONTEXT ( 'automotive_design' ) ;
#2308 = DIRECTION ( 'NONE',  ( 2.775557561562891351E-17, 1.000000000000000000, -8.326672684688671588E-17 ) ) ;
#2309 = CARTESIAN_POINT ( 'NONE',  ( 4.000000000000000000, -2.309401076758514915, -3.433295621305383349 ) ) ;
#2310 = CARTESIAN_POINT ( 'NONE',  ( -27.60187600103308014, 55.20208333237728482, -4.064049460664955760 ) ) ;
#2311 = CARTESIAN_POINT ( 'NONE',  ( 0.6937372685066666156, -4.453844082567737672, -3.610536846335894445 ) ) ;
#2312 = FACE_OUTER_BOUND ( 'NONE', #7167, .T. ) ;
#2313 = ORIENTED_EDGE ( 'NONE', *, *, #7841, .T. ) ;
#2314 = CARTESIAN_POINT ( 'NONE',  ( -1.734723475976807094E-15, 33.50000000000000000, 13.65625000000000355 ) ) ;
#2315 = PLANE ( 'NONE',  #9113 ) ;
#2316 = CARTESIAN_POINT ( 'NONE',  ( -26.25045812061784289, 13.49999999999941913, -5.000000000000000000 ) ) ;
#2317 = CARTESIAN_POINT ( 'NONE',  ( -27.60187600103308725, 53.62708333237728198, -4.064049460664955760 ) ) ;
#2318 = CARTESIAN_POINT ( 'NONE',  ( 22.88317621546045189, 19.71992003298075957, 12.00579112326941988 ) ) ;
#2319 = CARTESIAN_POINT ( 'NONE',  ( -23.98076211353314235, 50.19999999999986073, -5.000000000000103029 ) ) ;
#2320 = EDGE_LOOP ( 'NONE', ( #5295, #8237 ) ) ;
#2321 = CARTESIAN_POINT ( 'NONE',  ( -27.60187600103308014, 55.08541666571061057, -5.935950539335252074 ) ) ;
#2322 = ORIENTED_EDGE ( 'NONE', *, *, #6099, .F. ) ;
#2323 = ORIENTED_EDGE ( 'NONE', *, *, #3148, .F. ) ;
#2324 = CARTESIAN_POINT ( 'NONE',  ( 4.000000000000000000, -2.309401076758514915, -3.433295621305383349 ) ) ;
#2325 = ORIENTED_EDGE ( 'NONE', *, *, #107, .T. ) ;
#2326 = DIRECTION ( 'NONE',  ( -0.8660254037844377084, -0.5000000000000015543, 0.000000000000000000 ) ) ;
#2327 = EDGE_LOOP ( 'NONE', ( #2350, #6094, #6510, #2535 ) ) ;
#2328 = CIRCLE ( 'NONE', #9427, 2.149999999999992362 ) ;
#2329 = CARTESIAN_POINT ( 'NONE',  ( 18.76115673388714455, 17.03897527867736983, 11.01746215567925269 ) ) ;
#2330 = SURFACE_STYLE_FILL_AREA ( #6654 ) ;
#2331 = ADVANCED_FACE ( 'NONE', ( #10074 ), #6055, .T. ) ;
#2332 = CARTESIAN_POINT ( 'NONE',  ( 29.50000000000000711, 1.387778780781445676E-14, 17.49999999999999645 ) ) ;
#2333 = ADVANCED_FACE ( 'NONE', ( #5737 ), #7456, .F. ) ;
#2334 = CARTESIAN_POINT ( 'NONE',  ( 23.01143949934618504, 18.46103507366711227, 12.94889058896576906 ) ) ;
#2335 = CARTESIAN_POINT ( 'NONE',  ( -27.98076211353308551, 51.92083333142137036, -3.845299461620869330 ) ) ;
#2336 = CARTESIAN_POINT ( 'NONE',  ( 34.76713615931384993, 4.034733667027952997, -2.652855901285304796 ) ) ;
#2337 = CARTESIAN_POINT ( 'NONE',  ( 3.169801662054988700, 0.6882444255503921138, -3.499999999999999556 ) ) ;
#2338 = ORIENTED_EDGE ( 'NONE', *, *, #2197, .T. ) ;
#2339 = CARTESIAN_POINT ( 'NONE',  ( -3.500000000000003553, 31.44974746830583356, 13.89062500000000355 ) ) ;
#2340 = ORIENTED_EDGE ( 'NONE', *, *, #3572, .T. ) ;
#2341 = CARTESIAN_POINT ( 'NONE',  ( 22.32737213215407479, 19.20149278331202325, 13.00425721518307576 ) ) ;
#2342 = EDGE_CURVE ( 'NONE', #1362, #1687, #195, .T. ) ;
#2343 = CARTESIAN_POINT ( 'NONE',  ( 2.500000000000000000, 2.357898499370433054, -1.951563910473907981E-15 ) ) ;
#2344 = CARTESIAN_POINT ( 'NONE',  ( 34.74418829745650328, 4.228279689541293962, 2.594445730714923126 ) ) ;
#2345 = AXIS2_PLACEMENT_3D ( 'NONE', #2543, #10988, #8425 ) ;
#2346 = CARTESIAN_POINT ( 'NONE',  ( -26.85260690424861707, 57.49300631261340300, -3.199128986994839607 ) ) ;
#2347 = CARTESIAN_POINT ( 'NONE',  ( 3.527408190673962274, 28.61642175733934934, 13.51781658473306713 ) ) ;
#2348 = DIRECTION ( 'NONE',  ( -0.7071067811865405783, -0.7071067811865545671, 0.000000000000000000 ) ) ;
#2349 =( BOUNDED_CURVE ( )  B_SPLINE_CURVE ( 2, ( #10497, #7996, #8883, #4451, #2838, #1213, #9547, #6209, #2887 ),
 .UNSPECIFIED., .F., .F. ) 
 B_SPLINE_CURVE_WITH_KNOTS ( ( 3, 2, 2, 2, 3 ),
 ( 0.08333333333333338422, 0.09259259259259258745, 0.1111111111111111049, 0.1296296296296296224, 0.1388888888888888951 ),
 .UNSPECIFIED. ) 
 CURVE ( )  GEOMETRIC_REPRESENTATION_ITEM ( )  RATIONAL_B_SPLINE_CURVE ( ( 0.9330127018922194093, 0.9330127018922197424, 1.000000000000000000, 0.8660254037844387076, 1.000000000000000000, 0.8660254037844387076, 1.000000000000000000, 0.9330127018922191873, 0.9330127018922192983 ) ) 
 REPRESENTATION_ITEM ( '' )  );
#2350 = ORIENTED_EDGE ( 'NONE', *, *, #8304, .F. ) ;
#2351 = CARTESIAN_POINT ( 'NONE',  ( -26.98076211353309972, 55.24583333142137320, -6.732050807568954909 ) ) ;
#2352 = EDGE_CURVE ( 'NONE', #5059, #3529, #8459, .T. ) ;
#2353 = EDGE_LOOP ( 'NONE', ( #813, #1285, #3939, #4050, #1268 ) ) ;
#2354 = CARTESIAN_POINT ( 'NONE',  ( 2.521662442312485819, 32.42808502599335441, 15.74780841526694175 ) ) ;
#2355 = DIRECTION ( 'NONE',  ( 1.000000000000000000, 0.000000000000000000, 0.000000000000000000 ) ) ;
#2356 = FACE_OUTER_BOUND ( 'NONE', #2946, .T. ) ;
#2357 = DIRECTION ( 'NONE',  ( -0.000000000000000000, 0.000000000000000000, -1.000000000000000000 ) ) ;
#2358 = DIRECTION ( 'NONE',  ( -1.000000000000000000, -0.000000000000000000, -0.000000000000000000 ) ) ;
#2359 = CARTESIAN_POINT ( 'NONE',  ( -25.17020516978313083, 55.37708333237728198, -3.596074190997380349 ) ) ;
#2360 = ADVANCED_FACE ( 'NONE', ( #4245 ), #3127, .F. ) ;
#2361 = CARTESIAN_POINT ( 'NONE',  ( -25.98076211353311038, 61.49999999999985789, -8.500000000000694556 ) ) ;
#2362 = CARTESIAN_POINT ( 'NONE',  ( 4.000000000000000000, 0.8378280264232961239, -3.220590601395640018 ) ) ;
#2363 = ORIENTED_EDGE ( 'NONE', *, *, #4819, .F. ) ;
#2364 = CARTESIAN_POINT ( 'NONE',  ( -1.219727444046192735E-16, 2.000000000000000000, 5.500000000000000000 ) ) ;
#2365 = CARTESIAN_POINT ( 'NONE',  ( 0.000000000000000000, 0.000000000000000000, 0.000000000000000000 ) ) ;
#2366 = DIRECTION ( 'NONE',  ( 0.000000000000000000, 0.000000000000000000, 1.000000000000000000 ) ) ;
#2367 = CARTESIAN_POINT ( 'NONE',  ( -26.79131905728310059, 52.75208333237728198, -6.403925809002825709 ) ) ;
#2368 = CARTESIAN_POINT ( 'NONE',  ( 20.28019557727208166, 19.74811736329550982, 11.00732503135576401 ) ) ;
#2369 = CARTESIAN_POINT ( 'NONE',  ( -23.98076211353314235, 52.24166666666653924, -3.845299461620867554 ) ) ;
#2370 = VERTEX_POINT ( 'NONE', #9066 ) ;
#2371 = CARTESIAN_POINT ( 'NONE',  ( -25.98076211353311393, 55.66874999904395338, -6.871901078670400231 ) ) ;
#2372 = ORIENTED_EDGE ( 'NONE', *, *, #10918, .T. ) ;
#2373 = TOROIDAL_SURFACE ( 'NONE', #6995, 2.700000000000001066, 0.2000000000000000111 ) ;
#2374 = EDGE_LOOP ( 'NONE', ( #4836, #3850, #10797, #816, #117, #3301, #37, #1091, #9343, #10366, #204, #10004 ) ) ;
#2375 = CARTESIAN_POINT ( 'NONE',  ( -25.98076211353311038, 61.49999999999985789, -5.000000000000102141 ) ) ;
#2376 = ORIENTED_EDGE ( 'NONE', *, *, #4928, .T. ) ;
#2377 = LINE ( 'NONE', #7492, #3098 ) ;
#2378 = CARTESIAN_POINT ( 'NONE',  ( 0.000000000000000000, 0.000000000000000000, 0.000000000000000000 ) ) ;
#2379 = ORIENTED_EDGE ( 'NONE', *, *, #4794, .F. ) ;
#2380 = CARTESIAN_POINT ( 'NONE',  ( 16.89796509758404852, 18.05178237072099989, 12.14735994959144350 ) ) ;
#2381 = VECTOR ( 'NONE', #7355, 999.9999999999998863 ) ;
#2382 = EDGE_CURVE ( 'NONE', #6022, #381, #7696, .T. ) ;
#2383 = FACE_OUTER_BOUND ( 'NONE', #5884, .T. ) ;
#2384 = VECTOR ( 'NONE', #9155, 1000.000000000000000 ) ;
#2385 = DIRECTION ( 'NONE',  ( 1.000000000000000000, 0.000000000000000000, 0.000000000000000000 ) ) ;
#2386 = CARTESIAN_POINT ( 'NONE',  ( 21.33873319047917150, 17.29751440752404434, 12.94889058896590583 ) ) ;
#2387 = CARTESIAN_POINT ( 'NONE',  ( -23.98076211353314235, 52.91249999808803040, -5.000000000000103029 ) ) ;
#2388 = CIRCLE ( 'NONE', #2941, 2.100000000000000089 ) ;
#2389 = CARTESIAN_POINT ( 'NONE',  ( 4.000000000000000000, 0.000000000000000000, 0.000000000000000000 ) ) ;
#2390 = LINE ( 'NONE', #9224, #4040 ) ;
#2391 = ORIENTED_EDGE ( 'NONE', *, *, #10554, .F. ) ;
#2392 = VECTOR ( 'NONE', #1632, 1000.000000000000000 ) ;
#2393 = CARTESIAN_POINT ( 'NONE',  ( -3.500000000000005329, 30.06616922564516869, 14.96655841526694175 ) ) ;
#2394 = VECTOR ( 'NONE', #10448, 1000.000000000000000 ) ;
#2395 = ORIENTED_EDGE ( 'NONE', *, *, #10128, .T. ) ;
#2396 = EDGE_CURVE ( 'NONE', #6934, #7320, #10806, .T. ) ;
#2397 = CARTESIAN_POINT ( 'NONE',  ( 21.41520517525563605, 22.70178780811528441, 13.00425721518307753 ) ) ;
#2398 = EDGE_CURVE ( 'NONE', #10879, #8683, #9078, .T. ) ;
#2399 = AXIS2_PLACEMENT_3D ( 'NONE', #7239, #8226, #3126 ) ;
#2400 = DIRECTION ( 'NONE',  ( -1.000000000000000000, -0.000000000000000000, -0.000000000000000000 ) ) ;
#2401 = DIRECTION ( 'NONE',  ( -0.5000000000000019984, -0.8660254037844375974, 0.000000000000000000 ) ) ;
#2403 = DIRECTION ( 'NONE',  ( -1.000000000000000000, -6.098637220230963674E-17, -1.156482317317871478E-16 ) ) ;
#2402 = CIRCLE ( 'NONE', #10922, 24.99999999999999645 ) ;
#2404 = CARTESIAN_POINT ( 'NONE',  ( -1.515916693951010252, 33.47259180932604750, 15.23656658473306535 ) ) ;
#2405 = PLANE ( 'NONE',  #8449 ) ;
#2406 = EDGE_LOOP ( 'NONE', ( #1931, #8109, #8691, #3615 ) ) ;
#2407 = CYLINDRICAL_SURFACE ( 'NONE', #9005, 4.999999999999997335 ) ;
#2408 = ORIENTED_EDGE ( 'NONE', *, *, #4921, .T. ) ;
#2409 = EDGE_CURVE ( 'NONE', #4976, #7117, #5094, .T. ) ;
#2410 = EDGE_LOOP ( 'NONE', ( #2733, #5468, #10851, #4676 ) ) ;
#2411 = DIRECTION ( 'NONE',  ( 0.000000000000000000, 0.000000000000000000, 1.000000000000000000 ) ) ;
#2412 = AXIS2_PLACEMENT_3D ( 'NONE', #9025, #1415, #4808 ) ;
#2413 = B_SPLINE_CURVE_WITH_KNOTS ( 'NONE', 3,
 ( #3775, #8770, #324, #7157, #7890 ),
 .UNSPECIFIED., .F., .F.,
 ( 4, 1, 4 ),
 ( 0.000000000000000000, 0.002309401076758505356, 0.004618802153517010713 ),
 .UNSPECIFIED. ) ;
#2414 = DIRECTION ( 'NONE',  ( 1.000000000000000000, -0.000000000000000000, 1.156482317317871478E-16 ) ) ;
#2415 = CARTESIAN_POINT ( 'NONE',  ( 18.10462311893278553, 17.05669763433401087, 12.04589798090090902 ) ) ;
#2416 = LINE ( 'NONE', #9811, #4894 ) ;
#2417 = EDGE_CURVE ( 'NONE', #7830, #9083, #4094, .T. ) ;
#2418 = ADVANCED_FACE ( 'NONE', ( #5036 ), #1276, .F. ) ;
#2419 = CARTESIAN_POINT ( 'NONE',  ( 34.94281041931228771, 2.000000000000002220, 5.500000000000000000 ) ) ;
#2420 = CARTESIAN_POINT ( 'NONE',  ( -27.60187600103308370, 55.14374999904394059, -5.000000000000103029 ) ) ;
#2421 = CARTESIAN_POINT ( 'NONE',  ( -21.21106610644865498, 13.49999999999941913, -9.500000000000000000 ) ) ;
#2422 = CARTESIAN_POINT ( 'NONE',  ( 3.200000000000000178, 0.000000000000000000, 0.000000000000000000 ) ) ;
#2423 = ORIENTED_EDGE ( 'NONE', *, *, #8672, .T. ) ;
#2424 = CARTESIAN_POINT ( 'NONE',  ( -1.449747468305830678, 26.49999999999999289, 14.20312500000000355 ) ) ;
#2425 = CARTESIAN_POINT ( 'NONE',  ( -1.767766952966370209, 28.23223304703362402, 14.12500000000000355 ) ) ;
#2426 = DIRECTION ( 'NONE',  ( 0.000000000000000000, 0.000000000000000000, 1.000000000000000000 ) ) ;
#2427 = CARTESIAN_POINT ( 'NONE',  ( -27.60187600103308725, 50.30208333237727913, -4.064049460664955760 ) ) ;
#2428 = CARTESIAN_POINT ( 'NONE',  ( -24.35964822603314772, 53.16041666571062052, -4.064049460664953983 ) ) ;
#2429 = CARTESIAN_POINT ( 'NONE',  ( 21.42382487881899777, 22.58916947935290764, 11.00732503135576401 ) ) ;
#2430 = VECTOR ( 'NONE', #4581, 1000.000000000000000 ) ;
#2431 = AXIS2_PLACEMENT_3D ( 'NONE', #1550, #8326, #4221 ) ;
#2432 = CARTESIAN_POINT ( 'NONE',  ( -23.98076211353314235, 52.99999999999986500, -5.000000000000103029 ) ) ;
#2433 = EDGE_CURVE ( 'NONE', #3779, #3173, #8544, .T. ) ;
#2434 = VERTEX_POINT ( 'NONE', #2478 ) ;
#2435 = ADVANCED_FACE ( 'NONE', ( #10143 ), #10916, .F. ) ;
#2436 = VERTEX_POINT ( 'NONE', #735 ) ;
#2437 = EDGE_LOOP ( 'NONE', ( #7777, #6794 ) ) ;
#2438 = CARTESIAN_POINT ( 'NONE',  ( -6.015568632492068524, 34.47916666666665719, -2.499999999999998668 ) ) ;
#2439 = EDGE_LOOP ( 'NONE', ( #4240, #4235, #811, #836 ) ) ;
#2440 = CARTESIAN_POINT ( 'NONE',  ( 21.21106610644839208, 53.49999999999983658, 14.50000000000000000 ) ) ;
#2441 = DIRECTION ( 'NONE',  ( 6.982962677686266711E-15, 0.000000000000000000, -1.000000000000000000 ) ) ;
#2442 = ORIENTED_EDGE ( 'NONE', *, *, #1216, .T. ) ;
#2444 = CARTESIAN_POINT ( 'NONE',  ( 17.82405332881840110, 17.21173750719964346, 11.06307126761931769 ) ) ;
#2443 = VECTOR ( 'NONE', #8893, 1000.000000000000000 ) ;
#2445 = AXIS2_PLACEMENT_3D ( 'NONE', #8555, #4162, #2385 ) ;
#2446 = SURFACE_STYLE_FILL_AREA ( #4059 ) ;
#2447 = DIRECTION ( 'NONE',  ( -1.000000000000000000, -2.775557561562891351E-15, 0.000000000000000000 ) ) ;
#2448 = CARTESIAN_POINT ( 'NONE',  ( 12.00000000000000000, 1.610000000000000098, 0.000000000000000000 ) ) ;
#2449 = CARTESIAN_POINT ( 'NONE',  ( 19.79543838746868190, 16.23930471839911149, 12.94973781945951785 ) ) ;
#2450 = CARTESIAN_POINT ( 'NONE',  ( 11.61000000000001542, 0.000000000000000000, 2.000000000000000888 ) ) ;
#2451 = CARTESIAN_POINT ( 'NONE',  ( -24.98076211353313170, 55.59583333142136752, -3.267949192431250705 ) ) ;
#2452 = MECHANICAL_DESIGN_GEOMETRIC_PRESENTATION_REPRESENTATION (  '', ( #4953 ), #5300 ) ;
#2453 = COLOUR_RGB ( '', 0.40784314, 0.44705882, 0.49803922) ;
#2454 = CARTESIAN_POINT ( 'NONE',  ( -4.197393957002303999, 0.4069871074557429025, -3.503767560748926257 ) ) ;
#2455 = ORIENTED_EDGE ( 'NONE', *, *, #6340, .F. ) ;
#2456 = LINE ( 'NONE', #505, #5292 ) ;
#2457 = PRODUCT_DEFINITION_CONTEXT ( 'detailed design', #4593, 'design' ) ;
#2458 = VERTEX_POINT ( 'NONE', #9922 ) ;
#2459 = TOROIDAL_SURFACE ( 'NONE', #1564, 3.299999999999999822, 0.2000000000000000111 ) ;
#2460 = CARTESIAN_POINT ( 'NONE',  ( 2.474873734152922111, 27.52512626584708144, 14.43750000000000178 ) ) ;
#2461 = ORIENTED_EDGE ( 'NONE', *, *, #2089, .F. ) ;
#2462 = CARTESIAN_POINT ( 'NONE',  ( 22.73223279825284848, 19.49146071982302075, 13.00425721518307753 ) ) ;
#2463 = CARTESIAN_POINT ( 'NONE',  ( 21.30711663910541276, 17.34296610691914253, 11.95042449705224819 ) ) ;
#2464 = CIRCLE ( 'NONE', #2117, 1.500000000000001332 ) ;
#2465 = CARTESIAN_POINT ( 'NONE',  ( 0.000000000000000000, 30.00000000000000000, 2.500000000000000000 ) ) ;
#2466 = CARTESIAN_POINT ( 'NONE',  ( -24.98076211353213694, 57.99999999999985789, -9.000000000000701661 ) ) ;
#2467 = CARTESIAN_POINT ( 'NONE',  ( -2.428085025993349078, 27.47833755768751374, 13.12719158473306535 ) ) ;
#2468 = FACE_OUTER_BOUND ( 'NONE', #8896, .T. ) ;
#2469 = CARTESIAN_POINT ( 'NONE',  ( 0.02993401039711700642, -2.688325911136495883, 2.343682934607659529 ) ) ;
#2470 = PLANE ( 'NONE',  #4212 ) ;
#2471 = ORIENTED_EDGE ( 'NONE', *, *, #10105, .T. ) ;
#2472 = ORIENTED_EDGE ( 'NONE', *, *, #5726, .T. ) ;
#2473 = CARTESIAN_POINT ( 'NONE',  ( -25.98076211353311393, 52.12499999999985079, -3.000000000000132339 ) ) ;
#2474 = CARTESIAN_POINT ( 'NONE',  ( 0.000000000000000000, 3.031088913245510774, -1.750000000000042411 ) ) ;
#2475 = CARTESIAN_POINT ( 'NONE',  ( 19.84380896203909828, 21.37294244821887546, 12.00579112326902731 ) ) ;
#2476 = CARTESIAN_POINT ( 'NONE',  ( 2.500000000000007550, 31.03553390593274486, 14.67187500000000178 ) ) ;
#2477 = EDGE_CURVE ( 'NONE', #9793, #4773, #1728, .T. ) ;
#2478 = CARTESIAN_POINT ( 'NONE',  ( -26.25045812061784289, 16.50000000000026290, -9.500000000000000000 ) ) ;
#2479 = CARTESIAN_POINT ( 'NONE',  ( -27.60187600103308014, 51.41041666571062052, -5.935950539335252074 ) ) ;
#2480 = EDGE_CURVE ( 'NONE', #2061, #7117, #9781, .T. ) ;
#2481 = CYLINDRICAL_SURFACE ( 'NONE', #1211, 3.249999999999998224 ) ;
#2482 = CARTESIAN_POINT ( 'NONE',  ( 34.99999999999999289, -7.999999999999996447, 17.50000000000000355 ) ) ;
#2483 = EDGE_LOOP ( 'NONE', ( #6153, #4477, #810 ) ) ;
#2484 = CARTESIAN_POINT ( 'NONE',  ( 1.035533905932737975, 32.50000000000000711, 13.57812500000000178 ) ) ;
#2485 = CARTESIAN_POINT ( 'NONE',  ( -4.000000000000000000, 2.309401076758498483, -3.433295621305379353 ) ) ;
#2486 = CARTESIAN_POINT ( 'NONE',  ( -27.60187600103308725, 54.38541666571060773, -5.935950539335252074 ) ) ;
#2487 = CARTESIAN_POINT ( 'NONE',  ( -25.17020516978313083, 53.10208333237728340, -3.596074190997380349 ) ) ;
#2488 = CARTESIAN_POINT ( 'NONE',  ( 20.00651627240589647, 19.97666299463432438, 12.00579112326824216 ) ) ;
#2489 = CARTESIAN_POINT ( 'NONE',  ( -25.98076211353311393, 51.07499999999986784, -7.309401076758571314 ) ) ;
#2490 = EDGE_LOOP ( 'NONE', ( #9650, #9091 ) ) ;
#2491 = ORIENTED_EDGE ( 'NONE', *, *, #772, .F. ) ;
#2492 = ORIENTED_EDGE ( 'NONE', *, *, #6360, .F. ) ;
#2493 = DIRECTION ( 'NONE',  ( -1.000000000000000000, 0.000000000000000000, 0.000000000000000000 ) ) ;
#2494 = VERTEX_POINT ( 'NONE', #4136 ) ;
#2495 = CARTESIAN_POINT ( 'NONE',  ( 2.500000000000000000, -1.178949249685213863, 2.042000000000002924 ) ) ;
#2496 = DIRECTION ( 'NONE',  ( 0.000000000000000000, 0.000000000000000000, 1.000000000000000000 ) ) ;
#2497 = ORIENTED_EDGE ( 'NONE', *, *, #5677, .F. ) ;
#2498 = CARTESIAN_POINT ( 'NONE',  ( 19.92593468680574986, 17.66592327340909918, 11.00732503135576401 ) ) ;
#2499 = DIRECTION ( 'NONE',  ( 0.000000000000000000, 0.000000000000000000, 1.000000000000000000 ) ) ;
#2500 = DIRECTION ( 'NONE',  ( -0.000000000000000000, 1.345283343056720273E-15, 1.000000000000000000 ) ) ;
#2501 = CARTESIAN_POINT ( 'NONE',  ( 21.07893270796819962, 17.11679519544646411, 12.94889058896590583 ) ) ;
#2502 = ADVANCED_FACE ( 'NONE', ( #1529 ), #3308, .T. ) ;
#2503 = DIRECTION ( 'NONE',  ( -1.000000000000000000, 0.000000000000000000, 0.000000000000000000 ) ) ;
#2504 = CARTESIAN_POINT ( 'NONE',  ( -24.98076211353312814, 55.82916666475470180, -6.732050807568954909 ) ) ;
#2505 = DIRECTION ( 'NONE',  ( -1.000000000000000000, -0.000000000000000000, -0.000000000000000000 ) ) ;
#2506 = ORIENTED_EDGE ( 'NONE', *, *, #2144, .T. ) ;
#2507 = CARTESIAN_POINT ( 'NONE',  ( -27.98076211353308551, 50.46249999808803466, -5.000000000000103029 ) ) ;
#2508 = VERTEX_POINT ( 'NONE', #7414 ) ;
#2509 = CARTESIAN_POINT ( 'NONE',  ( 1.383578242660657098, 33.52740819067396671, 12.58031658473306713 ) ) ;
#2510 = VERTEX_POINT ( 'NONE', #4929 ) ;
#2511 = CARTESIAN_POINT ( 'NONE',  ( 15.22014049957087956, 18.31539340636219393, 13.24059312800850030 ) ) ;
#2512 = AXIS2_PLACEMENT_3D ( 'NONE', #9590, #6092, #10439 ) ;
#2513 = CARTESIAN_POINT ( 'NONE',  ( 0.2704726383733979667, 0.000000000000000000, 0.000000000000000000 ) ) ;
#2514 = CARTESIAN_POINT ( 'NONE',  ( -4.000000000000000000, -2.309401076758512694, -5.000000000000000000 ) ) ;
#2515 = DIRECTION ( 'NONE',  ( -3.865177154555985764E-17, -0.7071067811865489050, 0.7071067811865462405 ) ) ;
#2516 = CARTESIAN_POINT ( 'NONE',  ( -1.767766952966375094, 31.76776695296636888, 15.06250000000000355 ) ) ;
#2517 = DIRECTION ( 'NONE',  ( -1.000000000000000000, -0.000000000000000000, -0.000000000000000000 ) ) ;
#2518 = DIRECTION ( 'NONE',  ( -1.000000000000000000, 0.000000000000000000, 0.000000000000000000 ) ) ;
#2519 = DIRECTION ( 'NONE',  ( 0.000000000000000000, 0.000000000000000000, -1.000000000000000000 ) ) ;
#2520 = EDGE_LOOP ( 'NONE', ( #5629, #8214, #10726, #5978 ) ) ;
#2521 = ORIENTED_EDGE ( 'NONE', *, *, #192, .F. ) ;
#2522 = DIRECTION ( 'NONE',  ( 0.000000000000000000, 0.000000000000000000, -1.000000000000000000 ) ) ;
#2523 = CARTESIAN_POINT ( 'NONE',  ( -4.000000000000000000, -7.806255641895631925E-15, -3.142992957459232350 ) ) ;
#2524 = PRODUCT_RELATED_PRODUCT_CATEGORY ( 'part', '', ( #5290 ) ) ;
#2525 = CARTESIAN_POINT ( 'NONE',  ( 34.93373351399775117, 2.154066368359275785, -4.530732988813361395 ) ) ;
#2526 = AXIS2_PLACEMENT_3D ( 'NONE', #10493, #8926, #363 ) ;
#2527 = ADVANCED_FACE ( 'NONE', ( #10030, #5804 ), #9190, .F. ) ;
#2528 = CYLINDRICAL_SURFACE ( 'NONE', #1346, 1.000000000000972333 ) ;
#2529 = UNCERTAINTY_MEASURE_WITH_UNIT (LENGTH_MEASURE( 1.000000000000000082E-05 ), #1114, 'distance_accuracy_value', 'NONE');
#2530 = CARTESIAN_POINT ( 'NONE',  ( -25.98076211353311038, 59.49999999999985789, -5.000000000000102141 ) ) ;
#2531 = CARTESIAN_POINT ( 'NONE',  ( -25.17020516978313083, 54.50208333237728198, -3.596074190997380349 ) ) ;
#2532 = DIRECTION ( 'NONE',  ( -0.4999999999999978906, 0.8660254037844399289, -2.143152199010143228E-16 ) ) ;
#2533 = CARTESIAN_POINT ( 'NONE',  ( -25.71414987012866504, 57.02732617680999994, -3.014027881576975876 ) ) ;
#2534 = CARTESIAN_POINT ( 'NONE',  ( 4.000000000000000000, -2.511475576507276042, -3.469253905236643565 ) ) ;
#2535 = ORIENTED_EDGE ( 'NONE', *, *, #6003, .F. ) ;
#2536 = AXIS2_PLACEMENT_3D ( 'NONE', #10062, #5128, #886 ) ;
#2537 = CARTESIAN_POINT ( 'NONE',  ( 11.61000000000001542, 2.449293598294707893E-16, -2.000000000000000888 ) ) ;
#2538 = CARTESIAN_POINT ( 'NONE',  ( 29.49999999999999645, -3.999999999999986233, -9.499999999999991118 ) ) ;
#2539 = EDGE_CURVE ( 'NONE', #9740, #10159, #686, .T. ) ;
#2540 = CARTESIAN_POINT ( 'NONE',  ( -25.98076211353310683, 53.21874999904395054, -3.128098921329806714 ) ) ;
#2541 = LINE ( 'NONE', #4385, #9312 ) ;
#2542 = EDGE_CURVE ( 'NONE', #7103, #3195, #2874, .T. ) ;
#2543 = CARTESIAN_POINT ( 'NONE',  ( 2.000000000000000000, 0.000000000000000000, 0.000000000000000000 ) ) ;
#2544 = CARTESIAN_POINT ( 'NONE',  ( -25.98076211353311393, 53.87499999999985789, -7.309401076758571314 ) ) ;
#2545 = ORIENTED_EDGE ( 'NONE', *, *, #2925, .F. ) ;
#2546 = ORIENTED_EDGE ( 'NONE', *, *, #1447, .T. ) ;
#2547 = VERTEX_POINT ( 'NONE', #5205 ) ;
#2548 = CARTESIAN_POINT ( 'NONE',  ( 16.63280437751621577, 18.31694309078998018, 13.17442390236345595 ) ) ;
#2549 = VERTEX_POINT ( 'NONE', #240 ) ;
#2550 = EDGE_CURVE ( 'NONE', #8234, #625, #7816, .T. ) ;
#2551 = CARTESIAN_POINT ( 'NONE',  ( 0.000000000000000000, 30.00000000000000000, -2.500000000000000000 ) ) ;
#2552 = ORIENTED_EDGE ( 'NONE', *, *, #73, .T. ) ;
#2553 = CARTESIAN_POINT ( 'NONE',  ( 22.60530603367148927, 19.52972610220585636, 11.00732503135576401 ) ) ;
#2554 = LINE ( 'NONE', #5939, #1507 ) ;
#2555 = B_SPLINE_CURVE_WITH_KNOTS ( 'NONE', 3,
 ( #2985, #5482, #5584, #562, #3751, #4596, #2029, #7137 ),
 .UNSPECIFIED., .F., .F.,
 ( 4, 2, 2, 4 ),
 ( 0.000000000000000000, 0.002450665683189820997, 0.003675998524784731495, 0.004901331366379641993 ),
 .UNSPECIFIED. ) ;
#2556 = DIRECTION ( 'NONE',  ( 0.000000000000000000, 0.000000000000000000, 1.000000000000000000 ) ) ;
#2557 = FACE_OUTER_BOUND ( 'NONE', #10081, .T. ) ;
#2558 = EDGE_CURVE ( 'NONE', #7683, #6952, #1862, .T. ) ;
#2559 = EDGE_CURVE ( 'NONE', #7845, #8932, #5973, .T. ) ;
#2560 = CARTESIAN_POINT ( 'NONE',  ( 20.49609864019753402, 16.84626017008312360, 10.95195840513859231 ) ) ;
#2561 = AXIS2_PLACEMENT_3D ( 'NONE', #1379, #3976, #10756 ) ;
#2562 = DIRECTION ( 'NONE',  ( 0.000000000000000000, 0.000000000000000000, -1.000000000000000000 ) ) ;
#2563 = CARTESIAN_POINT ( 'NONE',  ( -23.98076211353314235, 55.71249999808803466, -5.000000000000103029 ) ) ;
#2564 = DIRECTION ( 'NONE',  ( -1.000000000000000000, 0.000000000000000000, 0.000000000000000000 ) ) ;
#2565 = ORIENTED_EDGE ( 'NONE', *, *, #3436, .T. ) ;
#2566 = CARTESIAN_POINT ( 'NONE',  ( -25.98076211353311393, 52.12499999999985079, -3.000000000000132783 ) ) ;
#2567 = ORIENTED_EDGE ( 'NONE', *, *, #418, .T. ) ;
#2568 = CARTESIAN_POINT ( 'NONE',  ( -2.474873734152920335, 32.47487373415291501, 16.31250000000000355 ) ) ;
#2569 = AXIS2_PLACEMENT_3D ( 'NONE', #7253, #3189, #3038 ) ;
#2570 = ORIENTED_EDGE ( 'NONE', *, *, #1797, .T. ) ;
#2571 = CARTESIAN_POINT ( 'NONE',  ( 19.78966864679935611, 21.38900865752197689, 13.00425721518248956 ) ) ;
#2572 = SURFACE_SIDE_STYLE ('',( #7742 ) ) ;
#2573 = ADVANCED_FACE ( 'NONE', ( #965 ), #6231, .F. ) ;
#2574 = B_SPLINE_CURVE_WITH_KNOTS ( 'NONE', 3,
 ( #660, #3219, #6597, #2129, #1290, #5999 ),
 .UNSPECIFIED., .F., .F.,
 ( 4, 2, 4 ),
 ( -3.640115492409406142E-06, 0.0002066546034006526487, 0.0004169493222937146744 ),
 .UNSPECIFIED. ) ;
#2575 = CARTESIAN_POINT ( 'NONE',  ( 0.000000000000000000, 1.773042676681340524, -2.059984127722458425E-15 ) ) ;
#2576 = CARTESIAN_POINT ( 'NONE',  ( 21.41951502703731691, 22.64547864373410135, 12.00579112326941988 ) ) ;
#2577 = CARTESIAN_POINT ( 'NONE',  ( -25.98076211353311393, 52.69374999904394485, -6.871901078670400231 ) ) ;
#2578 = CIRCLE ( 'NONE', #2213, 2.041999999999999815 ) ;
#2579 = CARTESIAN_POINT ( 'NONE',  ( 2.500000000000010214, 28.96446609406726225, 15.76562500000000178 ) ) ;
#2580 = DIRECTION ( 'NONE',  ( 0.000000000000000000, -0.5000000000000121014, -0.8660254037844316022 ) ) ;
#2581 = AXIS2_PLACEMENT_3D ( 'NONE', #2597, #2674, #3609 ) ;
#2582 = CYLINDRICAL_SURFACE ( 'NONE', #9851, 2.149999999999987921 ) ;
#2583 = FACE_BOUND ( 'NONE', #10774, .T. ) ;
#2584 = ORIENTED_EDGE ( 'NONE', *, *, #1092, .F. ) ;
#2585 = EDGE_CURVE ( 'NONE', #6989, #2222, #21, .T. ) ;
#2586 = ORIENTED_EDGE ( 'NONE', *, *, #90, .T. ) ;
#2587 = CARTESIAN_POINT ( 'NONE',  ( 0.2500000000000002220, 0.000000000000000000, 0.000000000000000000 ) ) ;
#2588 = VECTOR ( 'NONE', #2556, 1000.000000000000000 ) ;
#2589 = FACE_OUTER_BOUND ( 'NONE', #2483, .T. ) ;
#2590 = CARTESIAN_POINT ( 'NONE',  ( 22.63806431670481700, 19.48506897666907989, 12.00579112326951758 ) ) ;
#2591 = UNCERTAINTY_MEASURE_WITH_UNIT (LENGTH_MEASURE( 1.000000000000000082E-05 ), #2637, 'distance_accuracy_value', 'NONE');
#2592 = AXIS2_PLACEMENT_3D ( 'NONE', #8307, #797, #10920 ) ;
#2593 = CARTESIAN_POINT ( 'NONE',  ( 2.500000000000007550, 31.03553390593274486, 15.92187500000000178 ) ) ;
#2594 = CARTESIAN_POINT ( 'NONE',  ( 2.500000000000000000, 2.357898499370433054, -1.951563910473907981E-15 ) ) ;
#2595 = CARTESIAN_POINT ( 'NONE',  ( -24.35964822603314772, 53.27708333237728056, -5.935950539335252074 ) ) ;
#2596 = CARTESIAN_POINT ( 'NONE',  ( 0.000000000000000000, 0.000000000000000000, -5.000000000000000888 ) ) ;
#2597 = CARTESIAN_POINT ( 'NONE',  ( -25.98076211353311393, 49.49999999999986500, -5.000000000000103029 ) ) ;
#2598 = CARTESIAN_POINT ( 'NONE',  ( 4.000000000000000000, -0.8732470631449981147, -3.223155494240760088 ) ) ;
#2599 = VERTEX_POINT ( 'NONE', #3423 ) ;
#2600 = AXIS2_PLACEMENT_3D ( 'NONE', #9069, #10796, #4973 ) ;
#2601 = CARTESIAN_POINT ( 'NONE',  ( 24.50857997860451931, -3.999999999999987121, -4.999999999999992006 ) ) ;
#2602 = EDGE_CURVE ( 'NONE', #1804, #4007, #7123, .T. ) ;
#2603 = CARTESIAN_POINT ( 'NONE',  ( -27.98076211353308551, 54.10833333333319928, -3.845299461620869330 ) ) ;
#2604 = CARTESIAN_POINT ( 'NONE',  ( -26.79131905728310059, 53.86041666571061626, -3.596074190997381237 ) ) ;
#2605 = CARTESIAN_POINT ( 'NONE',  ( -25.98076211353311393, 55.27499999999985647, -7.000000000000072831 ) ) ;
#2606 = CIRCLE ( 'NONE', #4010, 4.000000000000600409 ) ;
#2607 = CARTESIAN_POINT ( 'NONE',  ( 21.55579831881754416, 20.86490736922957367, 14.50000000000000000 ) ) ;
#2608 = CARTESIAN_POINT ( 'NONE',  ( -23.98076211353314235, 53.05833333333319501, -6.154700538379337615 ) ) ;
#2609 = VERTEX_POINT ( 'NONE', #1074 ) ;
#2610 = EDGE_LOOP ( 'NONE', ( #6270, #5692, #6112 ) ) ;
#2611 = CARTESIAN_POINT ( 'NONE',  ( 16.58601566935801586, 18.36373179894819074, 12.17661548709639696 ) ) ;
#2612 = ADVANCED_FACE ( 'NONE', ( #6080, #2817 ), #910, .F. ) ;
#2613 = ADVANCED_FACE ( 'NONE', ( #1811 ), #4484, .T. ) ;
#2614 = DIRECTION ( 'NONE',  ( 1.000000000000000000, 0.000000000000000000, 0.000000000000000000 ) ) ;
#2615 = DIRECTION ( 'NONE',  ( 1.000000000000000000, 0.000000000000000000, 0.000000000000000000 ) ) ;
#2616 = ORIENTED_EDGE ( 'NONE', *, *, #5161, .T. ) ;
#2617 = CARTESIAN_POINT ( 'NONE',  ( 22.69616945897178084, 19.53356342368596898, 12.00579112326941988 ) ) ;
#2618 = CARTESIAN_POINT ( 'NONE',  ( 3.861362476283255685, 2.629030857715988656, -3.671615880910370500 ) ) ;
#2619 = CARTESIAN_POINT ( 'NONE',  ( -24.98076211353313170, 54.28333333333319644, -3.267949192431250705 ) ) ;
#2620 = AXIS2_PLACEMENT_3D ( 'NONE', #4156, #4893, #815 ) ;
#2621 = PLANE ( 'NONE',  #10776 ) ;
#2622 = CARTESIAN_POINT ( 'NONE',  ( 21.79510105275299026, 17.74985623046760708, 10.95195840513859231 ) ) ;
#2623 = EDGE_CURVE ( 'NONE', #9740, #5796, #6861, .T. ) ;
#2624 = CARTESIAN_POINT ( 'NONE',  ( 1.047444401652940007E-13, 30.00000000000000000, -2.500000000000000000 ) ) ;
#2625 = EDGE_CURVE ( 'NONE', #5721, #2134, #3045, .T. ) ;
#2626 = CARTESIAN_POINT ( 'NONE',  ( -26.79131905728310059, 50.36041666571060915, -3.596074190997381237 ) ) ;
#2627 = CARTESIAN_POINT ( 'NONE',  ( -4.204015924366189871, 1.626724848190922446, -3.610627190413390419 ) ) ;
#2628 = ORIENTED_EDGE ( 'NONE', *, *, #8772, .T. ) ;
#2629 = CARTESIAN_POINT ( 'NONE',  ( -25.98076211353415843, 59.00000000000900968, -2.999999999996041389 ) ) ;
#2630 = PRODUCT_DEFINITION_SHAPE ( 'NONE', 'NONE',  #2815 ) ;
#2631 = ORIENTED_EDGE ( 'NONE', *, *, #5215, .F. ) ;
#2632 = AXIS2_PLACEMENT_3D ( 'NONE', #4250, #7750, #1065 ) ;
#2633 = PRESENTATION_LAYER_ASSIGNMENT (  '', '', ( #9360 ) ) ;
#2634 = CARTESIAN_POINT ( 'NONE',  ( -1.449747468305836229, 33.50000000000000000, 14.98437500000000711 ) ) ;
#2635 = ORIENTED_EDGE ( 'NONE', *, *, #421, .T. ) ;
#2636 = CARTESIAN_POINT ( 'NONE',  ( 22.43871220627207563, 23.52649944903870249, 11.95042449705224819 ) ) ;
#2637 =( LENGTH_UNIT ( ) NAMED_UNIT ( * ) SI_UNIT ( .MILLI., .METRE. ) );
#2638 = CARTESIAN_POINT ( 'NONE',  ( -24.98076211353213694, 58.13434381516401572, -6.732050807568384698 ) ) ;
#2639 = CIRCLE ( 'NONE', #663, 1.500000000000001332 ) ;
#2640 = CARTESIAN_POINT ( 'NONE',  ( 21.51635413324704160, 18.70478684647606826, 12.00579112326941988 ) ) ;
#2641 = CARTESIAN_POINT ( 'NONE',  ( -26.79131905728310059, 50.18541666571061199, -3.596074190997381237 ) ) ;
#2642 = VECTOR ( 'NONE', #8700, 1000.000000000000000 ) ;
#2643 = CARTESIAN_POINT ( 'NONE',  ( -2.385244779468109755E-15, 32.50000000000000711, 16.15625000000000355 ) ) ;
#2644 = DIRECTION ( 'NONE',  ( -0.000000000000000000, 0.000000000000000000, 1.000000000000000000 ) ) ;
#2645 = DIRECTION ( 'NONE',  ( 0.000000000000000000, 0.5000000000000012212, 0.8660254037844380415 ) ) ;
#2646 = VERTEX_POINT ( 'NONE', #10195 ) ;
#2647 = EDGE_LOOP ( 'NONE', ( #7608, #2672, #6760, #3825 ) ) ;
#2648 = CIRCLE ( 'NONE', #6900, 2.041999999999999815 ) ;
#2649 = CARTESIAN_POINT ( 'NONE',  ( 0.000000000000000000, 3.031088913245550742, 1.749999999999972466 ) ) ;
#2650 = CARTESIAN_POINT ( 'NONE',  ( -4.203934362469166963, -1.640673743454851286, -3.598432614606932756 ) ) ;
#2651 = CIRCLE ( 'NONE', #8852, 20.00000000000000355 ) ;
#2652 = CARTESIAN_POINT ( 'NONE',  ( 34.82492259089467979, 3.500278077966952228, -2.894288569839196690 ) ) ;
#2653 = DIRECTION ( 'NONE',  ( 0.000000000000000000, -1.224646799147353454E-16, 1.000000000000000000 ) ) ;
#2654 = CARTESIAN_POINT ( 'NONE',  ( -0.1410422978106123659, 4.700232962125094893, -3.687027686973624707 ) ) ;
#2655 = CARTESIAN_POINT ( 'NONE',  ( -25.17020516978313083, 53.80208333237728624, -3.596074190997380349 ) ) ;
#2656 = DIRECTION ( 'NONE',  ( 0.000000000000000000, 0.000000000000000000, 1.000000000000000000 ) ) ;
#2657 = DIRECTION ( 'NONE',  ( 1.000000000000000000, 0.000000000000000000, 0.000000000000000000 ) ) ;
#2658 = CARTESIAN_POINT ( 'NONE',  ( 3.078243469714899039, -2.351289329882112256, 2.927447417349546832 ) ) ;
#2659 = EDGE_LOOP ( 'NONE', ( #1178, #4674, #7916, #5071 ) ) ;
#2660 = CARTESIAN_POINT ( 'NONE',  ( 2.000000000000000000, -1.773042676681341856, 2.276824562219559311E-15 ) ) ;
#2661 = CARTESIAN_POINT ( 'NONE',  ( -26.98076211353309972, 50.43333333333319501, -6.732050807568954909 ) ) ;
#2662 = DIRECTION ( 'NONE',  ( -0.7071067811865306973, 8.659560562355138702E-17, -0.7071067811865643371 ) ) ;
#2663 = CARTESIAN_POINT ( 'NONE',  ( -24.35964822603314772, 53.33541666571061768, -4.064049460664953983 ) ) ;
#2664 = LINE ( 'NONE', #7771, #4542 ) ;
#2665 = FACE_OUTER_BOUND ( 'NONE', #7272, .T. ) ;
#2666 = CARTESIAN_POINT ( 'NONE',  ( 2.100000000000000089, 0.000000000000000000, -0.2800830152838844622 ) ) ;
#2667 = ORIENTED_EDGE ( 'NONE', *, *, #7486, .T. ) ;
#2668 = EDGE_LOOP ( 'NONE', ( #5565, #9709, #10121, #7284 ) ) ;
#2669 = CARTESIAN_POINT ( 'NONE',  ( 0.2182762428107343500, 1.693953258775802606, -3.499999999999999556 ) ) ;
#2670 = DIRECTION ( 'NONE',  ( 1.000000000000000000, 0.000000000000000000, 0.000000000000000000 ) ) ;
#2671 =( LENGTH_UNIT ( ) NAMED_UNIT ( * ) SI_UNIT ( .MILLI., .METRE. ) );
#2672 = ORIENTED_EDGE ( 'NONE', *, *, #2952, .T. ) ;
#2673 = CARTESIAN_POINT ( 'NONE',  ( 19.84380896203909828, 21.37294244821887546, 12.00579112326902731 ) ) ;
#2674 = DIRECTION ( 'NONE',  ( 0.000000000000000000, 1.000000000000000000, 0.000000000000000000 ) ) ;
#2675 = FACE_OUTER_BOUND ( 'NONE', #4152, .T. ) ;
#2676 = EDGE_CURVE ( 'NONE', #10106, #5275, #6133, .T. ) ;
#2677 = CARTESIAN_POINT ( 'NONE',  ( 23.79237391907785693, 22.55645663433636017, 11.95042449705224819 ) ) ;
#2678 = DIRECTION ( 'NONE',  ( 0.000000000000000000, 0.000000000000000000, -1.000000000000000000 ) ) ;
#2679 = CARTESIAN_POINT ( 'NONE',  ( -27.98076211353308551, 55.36249999808803324, -5.000000000000103029 ) ) ;
#2680 = CARTESIAN_POINT ( 'NONE',  ( 24.99999259214812142, 30.01924558493218598, 2.500000000000000000 ) ) ;
#2681 = ORIENTED_EDGE ( 'NONE', *, *, #2965, .F. ) ;
#2682 = CARTESIAN_POINT ( 'NONE',  ( 11.99999999999999645, 0.000000000000000000, 1.610000000000000098 ) ) ;
#2683 = ORIENTED_EDGE ( 'NONE', *, *, #2279, .T. ) ;
#2684 = CARTESIAN_POINT ( 'NONE',  ( 3.500000000000005329, 30.00000000000000000, 15.84375000000000355 ) ) ;
#2685 = ORIENTED_EDGE ( 'NONE', *, *, #5051, .T. ) ;
#2686 = CARTESIAN_POINT ( 'NONE',  ( 21.33748252609158058, 23.71725136694109892, 12.94889058896590583 ) ) ;
#2687 = EDGE_CURVE ( 'NONE', #1419, #5040, #10669, .T. ) ;
#2688 = ADVANCED_FACE ( 'NONE', ( #9748 ), #6356, .F. ) ;
#2689 = CARTESIAN_POINT ( 'NONE',  ( 20.52771519157129987, 16.80080847068802541, 11.95042449705224819 ) ) ;
#2690 = CARTESIAN_POINT ( 'NONE',  ( 20.43380676890320657, 22.25420293214091316, 12.00579112326941988 ) ) ;
#2691 = CARTESIAN_POINT ( 'NONE',  ( -27.60187600103308370, 50.06874999904395196, -5.000000000000103029 ) ) ;
#2692 = AXIS2_PLACEMENT_3D ( 'NONE', #5915, #9298, #6746 ) ;
#2693 = CARTESIAN_POINT ( 'NONE',  ( -1.101703131577916883, 32.47259180932605460, 15.23656658473306535 ) ) ;
#2694 = CYLINDRICAL_SURFACE ( 'NONE', #259, 1.649999999999995248 ) ;
#2695 = CARTESIAN_POINT ( 'NONE',  ( -25.98076211353324894, 14.99999999999984190, 2.500000000000000000 ) ) ;
#2696 = ORIENTED_EDGE ( 'NONE', *, *, #10557, .T. ) ;
#2697 = ORIENTED_EDGE ( 'NONE', *, *, #2687, .F. ) ;
#2698 = CARTESIAN_POINT ( 'NONE',  ( 18.27511531525127353, 17.01097670698189290, 12.03680973694848966 ) ) ;
#2699 = ADVANCED_FACE ( 'NONE', ( #6449 ), #15, .T. ) ;
#2700 = AXIS2_PLACEMENT_3D ( 'NONE', #2868, #400, #10585 ) ;
#2701 = FACE_OUTER_BOUND ( 'NONE', #9834, .T. ) ;
#2702 = CARTESIAN_POINT ( 'NONE',  ( 22.88317621546045189, 19.71992003298075957, 12.00579112326941988 ) ) ;
#2703 = CARTESIAN_POINT ( 'NONE',  ( -2.385244779468109755E-15, 32.50000000000000711, 14.90625000000000355 ) ) ;
#2704 = CARTESIAN_POINT ( 'NONE',  ( -27.69734467828301305, 55.55430429566774819, -4.173301533939525854 ) ) ;
#2705 = CARTESIAN_POINT ( 'NONE',  ( -27.60187600103308014, 54.21041666571061768, -5.935950539335252074 ) ) ;
#2706 = ADVANCED_FACE ( 'NONE', ( #8866 ), #5178, .T. ) ;
#2707 = LINE ( 'NONE', #7759, #6892 ) ;
#2708 = CARTESIAN_POINT ( 'NONE',  ( -25.10838757727078630, 57.49417738710737069, -3.199400465621848433 ) ) ;
#2709 = CARTESIAN_POINT ( 'NONE',  ( 0.000000000000000000, 0.000000000000000000, 0.000000000000000000 ) ) ;
#2710 = ORIENTED_EDGE ( 'NONE', *, *, #6636, .F. ) ;
#2711 = CARTESIAN_POINT ( 'NONE',  ( 4.200000000000001954, 0.000000000000000000, 0.000000000000000000 ) ) ;
#2712 = CARTESIAN_POINT ( 'NONE',  ( -1.035533905932742638, 32.50000000000000000, 16.23437500000000355 ) ) ;
#2713 = CARTESIAN_POINT ( 'NONE',  ( 4.553649124439118623E-15, 27.49999999999999289, 15.53125000000000355 ) ) ;
#2714 = AXIS2_PLACEMENT_3D ( 'NONE', #3816, #1143, #2883 ) ;
#2715 = CARTESIAN_POINT ( 'NONE',  ( -27.60187600103308725, 53.10208333237727629, -4.064049460664955760 ) ) ;
#2716 = ADVANCED_FACE ( 'NONE', ( #1128 ), #9959, .T. ) ;
#2717 = CARTESIAN_POINT ( 'NONE',  ( -24.98076211353313170, 50.78333333333319644, -3.267949192431250705 ) ) ;
#2718 = CARTESIAN_POINT ( 'NONE',  ( 34.99999999999987210, -3.999999999999989786, -4.999999999999999112 ) ) ;
#2719 = CARTESIAN_POINT ( 'NONE',  ( -26.98076211353309972, 54.16666666666652930, -3.267949192431252037 ) ) ;
#2720 = CIRCLE ( 'NONE', #6422, 2.649999999999992362 ) ;
#2721 = ORIENTED_EDGE ( 'NONE', *, *, #1586, .F. ) ;
#2722 = ORIENTED_EDGE ( 'NONE', *, *, #108, .T. ) ;
#2723 = FACE_BOUND ( 'NONE', #3713, .T. ) ;
#2724 = DIRECTION ( 'NONE',  ( 1.000000000000000000, 0.000000000000000000, 0.000000000000000000 ) ) ;
#2725 = APPLICATION_PROTOCOL_DEFINITION ( 'draft international standard', 'automotive_design', 1998, #10477 ) ;
#2726 = ORIENTED_EDGE ( 'NONE', *, *, #6807, .T. ) ;
#2727 = DIRECTION ( 'NONE',  ( 0.000000000000000000, 0.000000000000000000, -1.000000000000000000 ) ) ;
#2728 = CARTESIAN_POINT ( 'NONE',  ( -23.98076211353314235, 54.45833333333320070, -6.154700538379337615 ) ) ;
#2729 = CARTESIAN_POINT ( 'NONE',  ( 19.32754978430113368, 16.15626933694376888, 10.95875375162450638 ) ) ;
#2730 = DIRECTION ( 'NONE',  ( 0.000000000000000000, 0.000000000000000000, 1.000000000000000000 ) ) ;
#2731 = CARTESIAN_POINT ( 'NONE',  ( -27.60187600103308370, 52.34374999904394343, -5.000000000000103029 ) ) ;
#2732 = CARTESIAN_POINT ( 'NONE',  ( -25.98076211353311393, 54.48749999808803324, -7.000000000000072831 ) ) ;
#2733 = ORIENTED_EDGE ( 'NONE', *, *, #1179, .F. ) ;
#2734 = DIRECTION ( 'NONE',  ( -0.5000000000000051070, 1.060575238724903217E-16, -0.8660254037844355990 ) ) ;
#2735 = EDGE_LOOP ( 'NONE', ( #10556, #4511, #5328, #222, #174 ) ) ;
#2736 = CARTESIAN_POINT ( 'NONE',  ( 1.515916693951011140, 26.52740819067395250, 14.61156658473306713 ) ) ;
#2737 = ORIENTED_EDGE ( 'NONE', *, *, #429, .T. ) ;
#2738 = EDGE_CURVE ( 'NONE', #1491, #1362, #4642, .T. ) ;
#2739 = CARTESIAN_POINT ( 'NONE',  ( 20.52771519157129987, 16.80080847068802541, 11.95042449705224819 ) ) ;
#2740 =( NAMED_UNIT ( * ) SI_UNIT ( $, .STERADIAN. ) SOLID_ANGLE_UNIT ( ) );
#2741 = AXIS2_PLACEMENT_3D ( 'NONE', #1480, #4876, #478 ) ;
#2742 = DIRECTION ( 'NONE',  ( -1.000000000000000000, -0.000000000000000000, -0.000000000000000000 ) ) ;
#2743 = CARTESIAN_POINT ( 'NONE',  ( 17.65010306112908722, 17.31038946799904465, 12.07741653513508417 ) ) ;
#2744 = CARTESIAN_POINT ( 'NONE',  ( -27.60187600103308014, 50.71041666571061768, -5.935950539335252074 ) ) ;
#2745 = CARTESIAN_POINT ( 'NONE',  ( -4.101948962585906244, 2.368261337751074169, -3.681124513963621503 ) ) ;
#2746 = DIRECTION ( 'NONE',  ( -1.000000000000000000, 0.000000000000000000, 0.000000000000000000 ) ) ;
#2747 = DIRECTION ( 'NONE',  ( 0.5150380749100549327, 1.049727191138617956E-16, 0.8571673007021118895 ) ) ;
#2748 = EDGE_CURVE ( 'NONE', #8872, #9873, #1188, .T. ) ;
#2749 = ORIENTED_EDGE ( 'NONE', *, *, #10749, .F. ) ;
#2750 = ORIENTED_EDGE ( 'NONE', *, *, #8713, .T. ) ;
#2751 = AXIS2_PLACEMENT_3D ( 'NONE', #4502, #6320, #9712 ) ;
#2752 = ADVANCED_FACE ( 'NONE', ( #8966 ), #8190, .T. ) ;
#2753 = FACE_OUTER_BOUND ( 'NONE', #2121, .T. ) ;
#2754 = CARTESIAN_POINT ( 'NONE',  ( 29.49999999999999645, -3.999999999999986233, -4.999999999999991118 ) ) ;
#2755 = CIRCLE ( 'NONE', #1145, 35.00000000000000000 ) ;
#2756 = DIRECTION ( 'NONE',  ( 1.000000000000000000, -0.000000000000000000, -0.000000000000000000 ) ) ;
#2757 = DIRECTION ( 'NONE',  ( 1.000000000000000000, 6.098637220230963674E-17, 1.156482317317871725E-16 ) ) ;
#2758 = CARTESIAN_POINT ( 'NONE',  ( -26.79131905728310059, 52.05208333237728624, -6.403925809002825709 ) ) ;
#2759 = AXIS2_PLACEMENT_3D ( 'NONE', #6047, #4281, #4224 ) ;
#2760 = CARTESIAN_POINT ( 'NONE',  ( 8.000000000000000000, -1.423651904008798069E-15, 0.000000000000000000 ) ) ;
#2761 = LINE ( 'NONE', #8645, #3996 ) ;
#2762 = EDGE_CURVE ( 'NONE', #2239, #2510, #2801, .T. ) ;
#2763 = VERTEX_POINT ( 'NONE', #3076 ) ;
#2764 = CARTESIAN_POINT ( 'NONE',  ( 4.750000000000000888, 0.000000000000000000, 0.000000000000000000 ) ) ;
#2765 = AXIS2_PLACEMENT_3D ( 'NONE', #6720, #4694, #2499 ) ;
#2766 = CARTESIAN_POINT ( 'NONE',  ( -0.9693646802875689472, 32.52740819067395961, 14.73218341526694175 ) ) ;
#2767 = AXIS2_PLACEMENT_3D ( 'NONE', #340, #390, #4687 ) ;
#2768 = CARTESIAN_POINT ( 'NONE',  ( -1.767766952966375094, 31.76776695296636888, 16.31250000000000355 ) ) ;
#2769 = UNCERTAINTY_MEASURE_WITH_UNIT (LENGTH_MEASURE( 1.000000000000000082E-05 ), #10761, 'distance_accuracy_value', 'NONE');
#2770 = CIRCLE ( 'NONE', #7047, 30.00000000000000000 ) ;
#2771 = ADVANCED_FACE ( 'NONE', ( #7925 ), #1087, .T. ) ;
#2772 = EDGE_CURVE ( 'NONE', #10106, #1168, #9798, .T. ) ;
#2773 = CARTESIAN_POINT ( 'NONE',  ( -23.98076211353314235, 55.01249999808803182, -5.000000000000103029 ) ) ;
#2774 = DIRECTION ( 'NONE',  ( -0.000000000000000000, 0.000000000000000000, 1.000000000000000000 ) ) ;
#2775 = TOROIDAL_SURFACE ( 'NONE', #7372, 5.384454397937118664, 0.5155456020628804703 ) ;
#2776 = CARTESIAN_POINT ( 'NONE',  ( 0.1217565302851224412, 2.351289329882196633, 2.927447417349528624 ) ) ;
#2777 = DIRECTION ( 'NONE',  ( 0.000000000000000000, 1.224646799147353207E-16, -1.000000000000000000 ) ) ;
#2778 = VECTOR ( 'NONE', #9473, 1000.000000000000000 ) ;
#2779 = VERTEX_POINT ( 'NONE', #3908 ) ;
#2780 = ORIENTED_EDGE ( 'NONE', *, *, #8807, .T. ) ;
#2781 = DIRECTION ( 'NONE',  ( -1.000000000000000000, 0.000000000000000000, 0.000000000000000000 ) ) ;
#2782 = CARTESIAN_POINT ( 'NONE',  ( 11.99999999999999645, 0.000000000000000000, 0.000000000000000000 ) ) ;
#2783 = ORIENTED_EDGE ( 'NONE', *, *, #5002, .F. ) ;
#2784 = DIRECTION ( 'NONE',  ( -0.000000000000000000, -0.000000000000000000, -1.000000000000000000 ) ) ;
#2785 = AXIS2_PLACEMENT_3D ( 'NONE', #9408, #7812, #9519 ) ;
#2786 = CARTESIAN_POINT ( 'NONE',  ( 0.000000000000000000, 0.000000000000000000, -4.974599999999998801 ) ) ;
#2787 = EDGE_CURVE ( 'NONE', #276, #4873, #7366, .T. ) ;
#2788 = CARTESIAN_POINT ( 'NONE',  ( 15.98809489411982199, 17.54743901181251786, 11.16417930307855677 ) ) ;
#2789 = CARTESIAN_POINT ( 'NONE',  ( 25.98076211353311749, 53.49999999999983658, 10.00000000000000178 ) ) ;
#2790 = CARTESIAN_POINT ( 'NONE',  ( -25.98076211353311393, 51.81874999904394485, -3.128098921329806714 ) ) ;
#2791 = DIRECTION ( 'NONE',  ( 1.000000000000000000, -0.000000000000000000, -0.000000000000000000 ) ) ;
#2792 = ORIENTED_EDGE ( 'NONE', *, *, #4741, .T. ) ;
#2793 = LINE ( 'NONE', #6222, #3521 ) ;
#2794 = AXIS2_PLACEMENT_3D ( 'NONE', #7301, #3868, #9758 ) ;
#2795 = ORIENTED_EDGE ( 'NONE', *, *, #6811, .F. ) ;
#2796 = CARTESIAN_POINT ( 'NONE',  ( 0.06616922564517943584, 27.49999999999998934, 14.53344158473306535 ) ) ;
#2797 = ORIENTED_EDGE ( 'NONE', *, *, #10906, .F. ) ;
#2798 = CARTESIAN_POINT ( 'NONE',  ( 21.04731615659443733, 17.16224689484156585, 11.95042449705224819 ) ) ;
#2799 = STYLED_ITEM ( 'NONE', ( #876 ), #4816 ) ;
#2800 = LINE ( 'NONE', #9618, #9007 ) ;
#2801 = B_SPLINE_CURVE_WITH_KNOTS ( 'NONE', 3,
 ( #2982, #4697, #8912, #1302, #9854, #10639, #455, #1358, #7242, #8805 ),
 .UNSPECIFIED., .F., .F.,
 ( 4, 2, 2, 2, 4 ),
 ( 0.000000000000000000, 0.0003977372743948460413, 0.0007954745487896920826, 0.001193211823184538124, 0.001590949097579384165 ),
 .UNSPECIFIED. ) ;
#2802 = CARTESIAN_POINT ( 'NONE',  ( 16.89796509758404852, 18.05178237072099989, 12.14735994959144350 ) ) ;
#2803 = CARTESIAN_POINT ( 'NONE',  ( -27.60187600103308014, 54.21041666571061768, -5.935950539335252074 ) ) ;
#2804 = CARTESIAN_POINT ( 'NONE',  ( 29.17190429162964094, 2.000000000000001776, 17.50099999999999767 ) ) ;
#2805 = AXIS2_PLACEMENT_3D ( 'NONE', #3700, #2192, #8085 ) ;
#2806 = VECTOR ( 'NONE', #8913, 1000.000000000000000 ) ;
#2807 = CARTESIAN_POINT ( 'NONE',  ( 2.000000000000000000, 0.000000000000000000, 0.000000000000000000 ) ) ;
#2808 = CARTESIAN_POINT ( 'NONE',  ( -25.44486372867087098, 52.76876073720499249, -3.000000000000133227 ) ) ;
#2809 = ORIENTED_EDGE ( 'NONE', *, *, #129, .F. ) ;
#2810 = ORIENTED_EDGE ( 'NONE', *, *, #2080, .T. ) ;
#2811 = CARTESIAN_POINT ( 'NONE',  ( 3.319999999999999840, 3.980102097228895766E-16, -3.249999999999998224 ) ) ;
#2812 = LINE ( 'NONE', #6188, #270 ) ;
#2813 = CIRCLE ( 'NONE', #1921, 2.500000000000001332 ) ;
#2814 = PRESENTATION_STYLE_ASSIGNMENT (( #4529 ) ) ;
#2815 = PRODUCT_DEFINITION ( 'UNKNOWN', '', #6336, #666 ) ;
#2816 = CARTESIAN_POINT ( 'NONE',  ( 27.50000000000001066, -3.999999999999986233, -9.499999999999991118 ) ) ;
#2817 = FACE_OUTER_BOUND ( 'NONE', #4834, .T. ) ;
#2818 = CARTESIAN_POINT ( 'NONE',  ( -25.98076211353311749, 56.99999999999886313, -3.000000000000122569 ) ) ;
#2819 = EDGE_CURVE ( 'NONE', #6817, #7809, #3179, .T. ) ;
#2820 = FILL_AREA_STYLE_COLOUR ( '', #8846 ) ;
#2821 = CARTESIAN_POINT ( 'NONE',  ( 3.500000000000005329, 30.00000000000000000, 14.59375000000000178 ) ) ;
#2822 = CARTESIAN_POINT ( 'NONE',  ( 29.49999999999999645, -3.999999999999983569, 10.00000000000000888 ) ) ;
#2823 = ORIENTED_EDGE ( 'NONE', *, *, #6898, .T. ) ;
#2824 = CARTESIAN_POINT ( 'NONE',  ( -25.98076211353311038, 60.99999999999985789, -9.000000000000701661 ) ) ;
#2825 = AXIS2_PLACEMENT_3D ( 'NONE', #1083, #7823, #355 ) ;
#2826 = CARTESIAN_POINT ( 'NONE',  ( 1.035533905932737975, 32.50000000000000711, 14.82812500000000178 ) ) ;
#2827 = CONICAL_SURFACE ( 'NONE', #3703, 3.499999999999999556, 1.047197551196603849 ) ;
#2828 = CARTESIAN_POINT ( 'NONE',  ( 4.198928548860774157, -0.8158838809860124996, -3.526471437616918170 ) ) ;
#2829 = CARTESIAN_POINT ( 'NONE',  ( -1.219727444046192735E-16, 2.000000000000000000, 0.000000000000000000 ) ) ;
#2830 = EDGE_CURVE ( 'NONE', #4665, #8097, #9676, .T. ) ;
#2831 = CARTESIAN_POINT ( 'NONE',  ( 0.000000000000000000, 3.031088913245510774, -1.750000000000042411 ) ) ;
#2832 = EDGE_CURVE ( 'NONE', #1717, #5040, #4828, .T. ) ;
#2833 = CARTESIAN_POINT ( 'NONE',  ( -24.35964822603314772, 51.35208333237728340, -5.935950539335252074 ) ) ;
#2834 = DIRECTION ( 'NONE',  ( -1.000000000000000000, -0.000000000000000000, -0.000000000000000000 ) ) ;
#2835 = DIRECTION ( 'NONE',  ( 1.000000000000000000, 0.000000000000000000, 0.000000000000000000 ) ) ;
#2836 = ORIENTED_EDGE ( 'NONE', *, *, #8107, .T. ) ;
#2837 = ORIENTED_EDGE ( 'NONE', *, *, #5493, .F. ) ;
#2838 = CARTESIAN_POINT ( 'NONE',  ( -23.98076211353314235, 50.81249999808803608, -5.000000000000103029 ) ) ;
#2839 = DIRECTION ( 'NONE',  ( 4.312387734421975743E-17, -0.7071067811865451302, -0.7071067811865500152 ) ) ;
#2840 = ADVANCED_BREP_SHAPE_REPRESENTATION ( '', ( #5541, #308 ), #10083 ) ;
#2841 = PRODUCT_CONTEXT ( 'NONE', #7412, 'mechanical' ) ;
#2842 = EDGE_LOOP ( 'NONE', ( #10161, #8175, #2423, #2303 ) ) ;
#2843 = DIRECTION ( 'NONE',  ( 0.000000000000000000, 0.000000000000000000, -1.000000000000000000 ) ) ;
#2844 =( BOUNDED_CURVE ( )  B_SPLINE_CURVE ( 2, ( #6630, #8309, #2314, #3254, #10811, #10036, #1429, #10755, #4824, #2424, #7421, #640, #9978, #6527, #5812, #5705, #9927, #9038, #5754, #3196, #578, #6577, #3974, #9084, #9139, #1479, #1535, #8253, #4938, #213, #1787, #5176, #272, #7730, #6002, #3454, #1049, #7000, #3612, #2002, #883 ),
 .UNSPECIFIED., .F., .T. ) 
 B_SPLINE_CURVE_WITH_KNOTS ( ( 3, 2, 2, 2, 2, 2, 2, 2, 2, 2, 2, 2, 2, 2, 2, 2, 2, 2, 2, 2, 3 ),
 ( -1.684088607864716175E-18, 0.04166666666666666435, 0.08333333333333332871, 0.1250000000000000000, 0.1666666666666666574, 0.2083333333333333148, 0.2500000000000000000, 0.2916666666666666852, 0.3333333333333333148, 0.3750000000000000000, 0.4166666666666666297, 0.4583333333333333148, 0.5000000000000000000, 0.5416666666666666297, 0.5833333333333333703, 0.6250000000000000000, 0.6666666666666666297, 0.7083333333333334814, 0.7500000000000000000, 0.7916666666666666297, 0.8001047462599640836 ),
 .UNSPECIFIED. ) 
 CURVE ( )  GEOMETRIC_REPRESENTATION_ITEM ( )  RATIONAL_B_SPLINE_CURVE ( ( 1.000000000000000000, 0.9238795325112867385, 1.000000000000000000, 0.9238795325112867385, 1.000000000000000000, 0.9238795325112867385, 1.000000000000000000, 0.9238795325112867385, 1.000000000000000000, 0.9238795325112867385, 1.000000000000000000, 0.9238795325112867385, 1.000000000000000000, 0.9238795325112867385, 1.000000000000000000, 0.9238795325112867385, 1.000000000000000000, 0.9238795325112867385, 1.000000000000000000, 0.9238795325112867385, 1.000000000000000000, 0.9238795325112867385, 1.000000000000000000, 0.9238795325112867385, 1.000000000000000000, 0.9238795325112867385, 1.000000000000000000, 0.9238795325112867385, 1.000000000000000000, 0.9238795325112867385, 1.000000000000000000, 0.9238795325112867385, 1.000000000000000000, 0.9238795325112867385, 1.000000000000000000, 0.9238795325112867385, 1.000000000000000000, 0.9238795325112867385, 1.000000000000000000, 0.9845845464796294522, 0.9754127805002987817 ) ) 
 REPRESENTATION_ITEM ( '' )  );
#2845 = DIRECTION ( 'NONE',  ( 1.000000000000000000, 0.000000000000000000, 0.000000000000000000 ) ) ;
#2846 = CARTESIAN_POINT ( 'NONE',  ( 23.74733166794916528, 22.52239063326518220, 10.95195840513859231 ) ) ;
#2847 = CARTESIAN_POINT ( 'NONE',  ( -25.98076211353311393, 49.49999999999986500, -7.000000000000074607 ) ) ;
#2848 = CARTESIAN_POINT ( 'NONE',  ( -24.35964822603314417, 51.99374999904394201, -5.000000000000103029 ) ) ;
#2849 = CARTESIAN_POINT ( 'NONE',  ( 0.3126073911696503060, 4.041451884327400101, -2.290628625700182053E-14 ) ) ;
#2850 = ORIENTED_EDGE ( 'NONE', *, *, #9742, .T. ) ;
#2851 = CARTESIAN_POINT ( 'NONE',  ( -25.98076211353311393, 54.83749999808803466, -3.000000000000132339 ) ) ;
#2852 = ORIENTED_EDGE ( 'NONE', *, *, #10099, .F. ) ;
#2853 = CARTESIAN_POINT ( 'NONE',  ( -2.500000000000003997, 29.93383077435482065, 14.22094158473306535 ) ) ;
#2854 = ORIENTED_EDGE ( 'NONE', *, *, #2676, .T. ) ;
#2855 = CARTESIAN_POINT ( 'NONE',  ( 18.94130700685887447, 16.00034706198404066, 11.96718634320919250 ) ) ;
#2856 = EDGE_CURVE ( 'NONE', #143, #9988, #777, .T. ) ;
#2857 = CARTESIAN_POINT ( 'NONE',  ( 29.17190429162964094, 7.000000000000002665, -2.500000000000000000 ) ) ;
#2858 = CARTESIAN_POINT ( 'NONE',  ( 21.04196501824306864, 22.63405165899350635, 13.00425721518307753 ) ) ;
#2859 = CARTESIAN_POINT ( 'NONE',  ( -23.98076211353314235, 49.49999999999986500, -5.000000000000103029 ) ) ;
#2860 = DIRECTION ( 'NONE',  ( -1.000000000000000000, -0.000000000000000000, -0.000000000000000000 ) ) ;
#2861 = CARTESIAN_POINT ( 'NONE',  ( 2.000000000000000000, -0.8865213383406694847, 1.535500000000001419 ) ) ;
#2862 = CARTESIAN_POINT ( 'NONE',  ( -26.24690541728881499, 58.97268535620265340, -6.985987684901640904 ) ) ;
#2863 = VERTEX_POINT ( 'NONE', #1412 ) ;
#2864 = DIRECTION ( 'NONE',  ( 1.000000000000000000, 0.000000000000000000, 0.000000000000000000 ) ) ;
#2865 = FACE_OUTER_BOUND ( 'NONE', #2250, .T. ) ;
#2866 = DIRECTION ( 'NONE',  ( -1.000000000000000000, 0.000000000000000000, 0.000000000000000000 ) ) ;
#2867 = CARTESIAN_POINT ( 'NONE',  ( 0.3126073911691547025, -2.020725942164465661, -3.499999999999999556 ) ) ;
#2868 = CARTESIAN_POINT ( 'NONE',  ( 2.550604951803072673, 0.000000000000000000, 0.000000000000000000 ) ) ;
#2869 = LINE ( 'NONE', #9694, #4763 ) ;
#2870 = CARTESIAN_POINT ( 'NONE',  ( -1.449747468305830678, 26.49999999999999289, 15.45312500000000178 ) ) ;
#2871 = CARTESIAN_POINT ( 'NONE',  ( -25.98076211353311393, 49.49999999999986500, -7.000000000000074607 ) ) ;
#2872 = EDGE_LOOP ( 'NONE', ( #3605, #3262, #56 ) ) ;
#2873 = DIRECTION ( 'NONE',  ( -0.000000000000000000, 0.000000000000000000, -1.000000000000000000 ) ) ;
#2874 = CIRCLE ( 'NONE', #712, 4.999999999999997335 ) ;
#2875 = CARTESIAN_POINT ( 'NONE',  ( 2.527408190673967159, 30.96936468028756906, 15.66968341526694175 ) ) ;
#2876 = CARTESIAN_POINT ( 'NONE',  ( 4.553649124439118623E-15, 27.49999999999999289, 14.28125000000000355 ) ) ;
#2877 = CARTESIAN_POINT ( 'NONE',  ( 23.04535143233503192, 19.92821688535955360, 12.00579112326941988 ) ) ;
#2878 = EDGE_CURVE ( 'NONE', #2239, #8562, #10127, .T. ) ;
#2879 = CARTESIAN_POINT ( 'NONE',  ( -25.98076211353311393, 55.18749999808803608, -7.000000000000072831 ) ) ;
#2880 = CARTESIAN_POINT ( 'NONE',  ( -25.98076211353311393, 53.78749999808803040, -7.000000000000072831 ) ) ;
#2881 = DIRECTION ( 'NONE',  ( -1.000000000000000000, -0.000000000000000000, -0.000000000000000000 ) ) ;
#2882 = CARTESIAN_POINT ( 'NONE',  ( -27.60187600103308370, 54.44374999904394485, -5.000000000000103029 ) ) ;
#2883 = DIRECTION ( 'NONE',  ( 0.000000000000000000, 0.000000000000000000, 1.000000000000000000 ) ) ;
#2884 = CYLINDRICAL_SURFACE ( 'NONE', #7299, 2.149999999999987921 ) ;
#2885 = ORIENTED_EDGE ( 'NONE', *, *, #953, .T. ) ;
#2886 = ORIENTED_EDGE ( 'NONE', *, *, #10498, .T. ) ;
#2887 = CARTESIAN_POINT ( 'NONE',  ( -25.98076211353311393, 50.98749999808804034, -7.000000000000073719 ) ) ;
#2888 = APPLICATION_CONTEXT ( 'automotive_design' ) ;
#2889 = EDGE_CURVE ( 'NONE', #3058, #7320, #2162, .T. ) ;
#2890 = DIRECTION ( 'NONE',  ( 0.000000000000000000, 0.000000000000000000, 1.000000000000000000 ) ) ;
#2891 = ITEM_DEFINED_TRANSFORMATION ( 'NONE', 'NONE', #10418,  #308 ) ;
#2892 = ORIENTED_EDGE ( 'NONE', *, *, #5196, .F. ) ;
#2893 = EDGE_CURVE ( 'NONE', #3442, #3173, #8183, .T. ) ;
#2894 = DIRECTION ( 'NONE',  ( 1.000000000000000000, 6.098637220230963674E-17, -0.000000000000000000 ) ) ;
#2895 = CARTESIAN_POINT ( 'NONE',  ( -24.35964822603314417, 50.41874999904395338, -5.000000000000103029 ) ) ;
#2896 = AXIS2_PLACEMENT_3D ( 'NONE', #5048, #6706, #1710 ) ;
#2897 = CARTESIAN_POINT ( 'NONE',  ( 17.40659673382103989, 17.54313596447427770, 11.09746175923963918 ) ) ;
#2898 = EDGE_LOOP ( 'NONE', ( #4680, #4279, #4909, #1485 ) ) ;
#2899 = CARTESIAN_POINT ( 'NONE',  ( -26.79131905728310059, 51.76041666571061484, -3.596074190997381237 ) ) ;
#2900 = EDGE_CURVE ( 'NONE', #8252, #8716, #2298, .T. ) ;
#2901 = VERTEX_POINT ( 'NONE', #3353 ) ;
#2902 = CARTESIAN_POINT ( 'NONE',  ( 26.25045812061784289, 0.000000000000000000, 14.50000000000000000 ) ) ;
#2903 = ORIENTED_EDGE ( 'NONE', *, *, #4860, .F. ) ;
#2904 = CARTESIAN_POINT ( 'NONE',  ( 1.767766952966372429, 31.76776695296637598, 14.75000000000000355 ) ) ;
#2905 = ORIENTED_EDGE ( 'NONE', *, *, #8772, .F. ) ;
#2906 = CARTESIAN_POINT ( 'NONE',  ( 19.86895450806392560, 16.41003605044161162, 10.95195963068177392 ) ) ;
#2907 = EDGE_CURVE ( 'NONE', #10134, #9486, #9248, .T. ) ;
#2908 = EDGE_CURVE ( 'NONE', #3474, #10992, #9421, .T. ) ;
#2909 = FACE_OUTER_BOUND ( 'NONE', #1547, .T. ) ;
#2910 = CARTESIAN_POINT ( 'NONE',  ( 20.76856923708738734, 18.11717751085002703, 13.00425721518307576 ) ) ;
#2911 = CARTESIAN_POINT ( 'NONE',  ( -27.60187600103308014, 53.62708333237728908, -4.064049460664955760 ) ) ;
#2912 = CARTESIAN_POINT ( 'NONE',  ( -31.74999999999995737, 4.286263797015736595E-16, -3.500000000000000000 ) ) ;
#2913 = DIRECTION ( 'NONE',  ( 6.098637220230963674E-17, -1.000000000000000000, 0.000000000000000000 ) ) ;
#2914 = DIRECTION ( 'NONE',  ( 1.000000000000000000, 6.098637220230963674E-17, 0.000000000000000000 ) ) ;
#2915 = VERTEX_POINT ( 'NONE', #1571 ) ;
#2916 = EDGE_LOOP ( 'NONE', ( #2274, #7235, #8984, #4264, #6768, #2885, #7111, #10354, #3084, #7563, #6085, #1163, #1003, #4364 ) ) ;
#2917 = CARTESIAN_POINT ( 'NONE',  ( 16.94475380574361623, 18.00499366256143219, 13.14516836485838169 ) ) ;
#2918 = DIRECTION ( 'NONE',  ( 1.000000000000000000, 0.000000000000000000, 0.000000000000000000 ) ) ;
#2919 = CARTESIAN_POINT ( 'NONE',  ( 2.000000000000000000, 1.773042676681340524, -2.059984127722458425E-15 ) ) ;
#2920 = DIRECTION ( 'NONE',  ( 0.000000000000000000, 0.000000000000000000, -1.000000000000000000 ) ) ;
#2921 = CARTESIAN_POINT ( 'NONE',  ( -6.259644161404860030E-16, -4.618802153517027165, -3.433295621305388234 ) ) ;
#2922 = CARTESIAN_POINT ( 'NONE',  ( 3.199999999999999734, 3.031088913245550742, 1.749999999999972466 ) ) ;
#2923 = CARTESIAN_POINT ( 'NONE',  ( -25.98076211353311393, 50.37499999999987210, -7.000000000000073719 ) ) ;
#2925 = EDGE_CURVE ( 'NONE', #5562, #4884, #4971, .T. ) ;
#2924 = CARTESIAN_POINT ( 'NONE',  ( -25.44486372867087098, 49.64373926088289579, -7.000000000000072831 ) ) ;
#2926 = CARTESIAN_POINT ( 'NONE',  ( 3.527408190673964494, 31.38357824266065776, 16.91968341526693820 ) ) ;
#2927 = LINE ( 'NONE', #4759, #5429 ) ;
#2928 = CIRCLE ( 'NONE', #3092, 1.999999999999971356 ) ;
#2929 = VERTEX_POINT ( 'NONE', #5689 ) ;
#2930 = LINE ( 'NONE', #2033, #4032 ) ;
#2931 = CARTESIAN_POINT ( 'NONE',  ( 1.814555661125939467, 31.72097824480680828, 14.49780841526694175 ) ) ;
#2932 = CARTESIAN_POINT ( 'NONE',  ( 1.767766952966372429, 31.76776695296637598, 16.00000000000000355 ) ) ;
#2933 = CARTESIAN_POINT ( 'NONE',  ( 19.69775075566884226, 17.43975236193677603, 12.00579112326941988 ) ) ;
#2934 = DIRECTION ( 'NONE',  ( 1.000000000000000000, -0.000000000000000000, -0.000000000000000000 ) ) ;
#2935 = AXIS2_PLACEMENT_3D ( 'NONE', #1718, #9488, #8378 ) ;
#2936 = CARTESIAN_POINT ( 'NONE',  ( -25.98076211353311393, 52.82499999999986784, -3.000000000000132339 ) ) ;
#2937 = DIRECTION ( 'NONE',  ( 0.000000000000000000, 0.000000000000000000, -1.000000000000000000 ) ) ;
#2938 = CARTESIAN_POINT ( 'NONE',  ( -25.98076211353311393, 52.51874999904395480, -3.128098921329806714 ) ) ;
#2939 = CARTESIAN_POINT ( 'NONE',  ( 0.000000000000000000, 3.031088913245550742, 1.749999999999972466 ) ) ;
#2940 = FACE_OUTER_BOUND ( 'NONE', #3397, .T. ) ;
#2941 = AXIS2_PLACEMENT_3D ( 'NONE', #1497, #6942, #6891 ) ;
#2942 = ORIENTED_EDGE ( 'NONE', *, *, #9479, .F. ) ;
#2943 = EDGE_CURVE ( 'NONE', #9728, #2779, #4480, .T. ) ;
#2944 = DIRECTION ( 'NONE',  ( 0.000000000000000000, 1.000000000000000000, 0.000000000000000000 ) ) ;
#2945 = CARTESIAN_POINT ( 'NONE',  ( -25.98076211353311038, 61.49999999999985789, -5.000000000000102141 ) ) ;
#2946 = EDGE_LOOP ( 'NONE', ( #2552, #5823, #2905, #2181, #1323, #5683 ) ) ;
#2947 = DIRECTION ( 'NONE',  ( -1.000000000000000000, 0.000000000000000000, 0.000000000000000000 ) ) ;
#2948 = VECTOR ( 'NONE', #10844, 1000.000000000000000 ) ;
#2949 = DIRECTION ( 'NONE',  ( -1.000000000000000000, 0.000000000000000000, 0.000000000000000000 ) ) ;
#2950 = AXIS2_PLACEMENT_3D ( 'NONE', #5326, #2835, #9036 ) ;
#2951 = CARTESIAN_POINT ( 'NONE',  ( 22.95140240311772573, 18.55416269319264444, 10.95195840513845553 ) ) ;
#2952 = EDGE_CURVE ( 'NONE', #4616, #2061, #559, .T. ) ;
#2953 = VERTEX_POINT ( 'NONE', #4915 ) ;
#2954 = CARTESIAN_POINT ( 'NONE',  ( -24.35964822603314772, 54.85208333237728340, -5.935950539335252074 ) ) ;
#2955 = AXIS2_PLACEMENT_3D ( 'NONE', #3350, #840, #3405 ) ;
#2956 = VERTEX_POINT ( 'NONE', #9912 ) ;
#2957 = DIRECTION ( 'NONE',  ( 0.000000000000000000, 0.000000000000000000, 1.000000000000000000 ) ) ;
#2958 = VERTEX_POINT ( 'NONE', #618 ) ;
#2959 = CARTESIAN_POINT ( 'NONE',  ( 2.527408190673965382, 29.03063531971243449, 13.51781658473306713 ) ) ;
#2960 = CIRCLE ( 'NONE', #3666, 2.000000000000000888 ) ;
#2961 = ORIENTED_EDGE ( 'NONE', *, *, #8615, .F. ) ;
#2962 = B_SPLINE_CURVE_WITH_KNOTS ( 'NONE', 3,
 ( #8531, #908, #9241, #4134, #2525, #4309, #7755, #7698, #3478, #7522, #6859, #2652, #6027, #10912, #4368, #6688, #9411, #8409 ),
 .UNSPECIFIED., .F., .F.,
 ( 4, 2, 2, 2, 2, 2, 2, 2, 4 ),
 ( 0.000000000000000000, 0.0005875687307069784411, 0.001175137461413956882, 0.001762706192120935648, 0.002350274922827915065, 0.002937843653534894482, 0.003525412384241873899, 0.004112981114948852449, 0.004700549845655830998 ),
 .UNSPECIFIED. ) ;
#2963 = CARTESIAN_POINT ( 'NONE',  ( 18.90462188152790901, 16.04371289204410189, 10.96879988954262153 ) ) ;
#2964 = ADVANCED_FACE ( 'NONE', ( #9117 ), #9962, .T. ) ;
#2965 = EDGE_CURVE ( 'NONE', #7506, #4391, #4648, .T. ) ;
#2966 = CARTESIAN_POINT ( 'NONE',  ( 19.38445574543743177, 22.63941596627307362, 11.95042449705263898 ) ) ;
#2967 = EDGE_CURVE ( 'NONE', #9280, #8338, #724, .T. ) ;
#2968 = CARTESIAN_POINT ( 'NONE',  ( 19.38642580597931087, 17.15576104669793267, 13.00425794126423362 ) ) ;
#2969 = AXIS2_PLACEMENT_3D ( 'NONE', #3135, #9030, #1421 ) ;
#2970 = LINE ( 'NONE', #1236, #672 ) ;
#2971 = CYLINDRICAL_SURFACE ( 'NONE', #5952, 2.149999999999988809 ) ;
#2972 = CARTESIAN_POINT ( 'NONE',  ( -23.98076211353314235, 52.91249999808803040, -5.000000000000103029 ) ) ;
#2973 = VERTEX_POINT ( 'NONE', #10900 ) ;
#2974 = ORIENTED_EDGE ( 'NONE', *, *, #3498, .T. ) ;
#2975 = CARTESIAN_POINT ( 'NONE',  ( 21.54797068462080745, 18.65933514708097007, 13.00425721518307576 ) ) ;
#2976 = B_SPLINE_CURVE_WITH_KNOTS ( 'NONE', 3,
 ( #7687, #3, #6786, #6015, #7570, #60, #3465, #8458, #7629, #10240, #9400, #1798, #5187, #8568, #950, #5023, #10295, #7744, #121, #3520, #6908, #2689, #8342, #10071, #2463, #5846, #9229, #1626, #775, #4182, #1233, #5349, #177, #7803, #1060, #5402, #7852, #3573, #1006, #5241, #7907, #4471, #6116, #7172, #10515, #1116, #2966, #2013, #226, #8786, #10568, #337 ),
 .UNSPECIFIED., .F., .F.,
 ( 4, 2, 2, 2, 2, 2, 2, 2, 2, 2, 2, 2, 2, 2, 2, 2, 2, 2, 2, 2, 2, 2, 2, 2, 2, 4 ),
 ( 0.05059550242215560267, 0.08415034466753366915, 0.1009277657902227232, 0.1177051869129117356, 0.1353321994545649831, 0.1529592119962182029, 0.1882132370795247256, 0.2234672621628312206, 0.2410942747044844681, 0.2587212872461377433, 0.2827395206008364026, 0.3067577539555350064, 0.3547942206649323249, 0.4028306873743295879, 0.4268489207290283027, 0.4508671540837269065, 0.4680275555186104164, 0.4851879569534939263, 0.5195087598232610571, 0.5881503655627953187, 0.6567919713023293582, 0.7254335770418635088, 0.7940751827813975483, 0.8627167885209316989, 0.9313583942604659605, 1.000000000000000000 ),
 .UNSPECIFIED. ) ;
#2977 = CARTESIAN_POINT ( 'NONE',  ( 0.000000000000000000, 0.000000000000000000, 0.000000000000000000 ) ) ;
#2978 = CARTESIAN_POINT ( 'NONE',  ( 0.3126073911691547025, -2.020725942164465661, -3.499999999999999556 ) ) ;
#2979 = DIRECTION ( 'NONE',  ( 1.000000000000000000, 0.000000000000000000, 0.000000000000000000 ) ) ;
#2980 = VECTOR ( 'NONE', #517, 1000.000000000000000 ) ;
#2981 = PRODUCT_DEFINITION_FORMATION_WITH_SPECIFIED_SOURCE ( 'ANY', '', #7066, .NOT_KNOWN. ) ;
#2982 = CARTESIAN_POINT ( 'NONE',  ( -24.98076211353213694, 57.99999999999985789, -6.732050807568384698 ) ) ;
#2983 = PLANE ( 'NONE',  #9729 ) ;
#2984 = CARTESIAN_POINT ( 'NONE',  ( 3.903127820947815962E-15, 26.49999999999999289, 15.53125000000000355 ) ) ;
#2985 = CARTESIAN_POINT ( 'NONE',  ( -4.211140560182196957, 2.431303136016537803, -3.745885042887433514 ) ) ;
#2986 = ORIENTED_EDGE ( 'NONE', *, *, #1972, .F. ) ;
#2987 = CARTESIAN_POINT ( 'NONE',  ( -3.500000000000005329, 30.06616922564516869, 17.46655841526694175 ) ) ;
#2988 = AXIS2_PLACEMENT_3D ( 'NONE', #10784, #1453, #5680 ) ;
#2989 = AXIS2_PLACEMENT_3D ( 'NONE', #9579, #241, #6242 ) ;
#2990 = CARTESIAN_POINT ( 'NONE',  ( 2.527408190673967159, 30.96936468028756906, 16.91968341526693820 ) ) ;
#2991 = CARTESIAN_POINT ( 'NONE',  ( 19.35452611835372849, 17.20101589911864437, 12.00579185514580338 ) ) ;
#2992 = CARTESIAN_POINT ( 'NONE',  ( -25.98076211353311393, 52.03749999808803750, -3.000000000000132339 ) ) ;
#2993 = DIRECTION ( 'NONE',  ( 1.000000000000000000, 0.000000000000000000, 0.000000000000000000 ) ) ;
#2994 = CARTESIAN_POINT ( 'NONE',  ( 0.02448733951239481094, 4.877042772274728044, -3.751161874094022242 ) ) ;
#2995 = CARTESIAN_POINT ( 'NONE',  ( -27.60187600103308014, 53.10208333237727629, -4.064049460664955760 ) ) ;
#2996 = EDGE_CURVE ( 'NONE', #5796, #10159, #3585, .T. ) ;
#2997 = CARTESIAN_POINT ( 'NONE',  ( -25.71106610644865498, 16.50000000000026290, -9.500000000000000000 ) ) ;
#2998 = VECTOR ( 'NONE', #767, 1000.000000000000000 ) ;
#2999 = CARTESIAN_POINT ( 'NONE',  ( -4.175002511812151873, -2.208363329454905877, -3.469254087858246738 ) ) ;
#3000 = EDGE_LOOP ( 'NONE', ( #9977, #1656, #1469, #5840, #10769, #4986 ) ) ;
#3001 = VECTOR ( 'NONE', #6082, 1000.000000000000227 ) ;
#3002 = ORIENTED_EDGE ( 'NONE', *, *, #761, .T. ) ;
#3003 = AXIS2_PLACEMENT_3D ( 'NONE', #9371, #3431, #6806 ) ;
#3004 = CARTESIAN_POINT ( 'NONE',  ( -27.78268512908116961, 55.49961679590672503, -4.132201955500060642 ) ) ;
#3005 = CARTESIAN_POINT ( 'NONE',  ( -25.17020516978313083, 51.00208333237728198, -3.596074190997380349 ) ) ;
#3006 = CARTESIAN_POINT ( 'NONE',  ( 24.04035011313704118, 22.03839429810881612, 10.95195840513898666 ) ) ;
#3007 = EDGE_LOOP ( 'NONE', ( #7531, #9665, #9846, #2007, #8858 ) ) ;
#3008 = CARTESIAN_POINT ( 'NONE',  ( 34.85586774767502050, 3.177316488306994646, 3.109148447068123655 ) ) ;
#3009 = ORIENTED_EDGE ( 'NONE', *, *, #3762, .F. ) ;
#3010 = LINE ( 'NONE', #1903, #3330 ) ;
#3011 = EDGE_LOOP ( 'NONE', ( #3530, #13, #10343, #1374 ) ) ;
#3012 = CARTESIAN_POINT ( 'NONE',  ( -1.035533905932742638, 32.50000000000000000, 13.73437500000000533 ) ) ;
#3013 =( NAMED_UNIT ( * ) PLANE_ANGLE_UNIT ( ) SI_UNIT ( $, .RADIAN. ) );
#3014 = VERTEX_POINT ( 'NONE', #8520 ) ;
#3015 = CARTESIAN_POINT ( 'NONE',  ( 23.74733166794916528, 22.52239063326518220, 10.95195840513859231 ) ) ;
#3016 = SHAPE_REPRESENTATION ( 'caliper arm left', ( #308 ), #10083 ) ;
#3017 =( LENGTH_UNIT ( ) NAMED_UNIT ( * ) SI_UNIT ( .MILLI., .METRE. ) );
#3018 = CARTESIAN_POINT ( 'NONE',  ( 11.99999999999999645, 2.210487472460973191E-16, -1.610000000000000098 ) ) ;
#3019 = CARTESIAN_POINT ( 'NONE',  ( 22.13583660366028738, 22.61346442202890472, 13.00425721518307753 ) ) ;
#3020 = CARTESIAN_POINT ( 'NONE',  ( -27.98076211353308551, 51.22083333142136752, -3.845299461620869330 ) ) ;
#3021 = LINE ( 'NONE', #10001, #1872 ) ;
#3022 = DIRECTION ( 'NONE',  ( -1.000000000000000000, 0.000000000000000000, 0.000000000000000000 ) ) ;
#3023 = EDGE_LOOP ( 'NONE', ( #9776, #1790, #2325, #7797 ) ) ;
#3024 = VERTEX_POINT ( 'NONE', #1913 ) ;
#3025 = ADVANCED_FACE ( 'NONE', ( #1800 ), #9931, .T. ) ;
#3026 = CARTESIAN_POINT ( 'NONE',  ( 19.35452611835372849, 17.20101589911864437, 12.00579185514580338 ) ) ;
#3027 = CARTESIAN_POINT ( 'NONE',  ( 2.000000000000000000, 0.8865213383406680414, -1.535500000000000975 ) ) ;
#3028 = CARTESIAN_POINT ( 'NONE',  ( 4.750000000000000888, -1.622657008870242882E-15, 0.000000000000000000 ) ) ;
#3029 = CARTESIAN_POINT ( 'NONE',  ( 0.000000000000000000, 0.000000000000000000, 0.000000000000000000 ) ) ;
#3030 = CARTESIAN_POINT ( 'NONE',  ( 0.000000000000000000, 30.00000000000000000, -23.71320343559643007 ) ) ;
#3031 = CARTESIAN_POINT ( 'NONE',  ( -1.515916693951010252, 33.47259180932604750, 12.73656658473306358 ) ) ;
#3032 = CYLINDRICAL_SURFACE ( 'NONE', #7369, 2.000000000000000888 ) ;
#3033 = ORIENTED_EDGE ( 'NONE', *, *, #242, .F. ) ;
#3034 = PRESENTATION_STYLE_ASSIGNMENT (( #3864 ) ) ;
#3035 = EDGE_CURVE ( 'NONE', #2915, #40, #1209, .T. ) ;
#3036 = CARTESIAN_POINT ( 'NONE',  ( 2.428085025993357071, 27.47833755768751374, 15.43530841526694175 ) ) ;
#3037 = CARTESIAN_POINT ( 'NONE',  ( 30.75045812061784289, 53.49999999999983658, 10.00000000000000178 ) ) ;
#3038 = DIRECTION ( 'NONE',  ( 0.7512361908166128588, 0.6577071706380231975, 0.05536662621716938876 ) ) ;
#3039 = CARTESIAN_POINT ( 'NONE',  ( 2.000000000000000000, -0.8865213383406694847, 1.535500000000001419 ) ) ;
#3040 = ADVANCED_FACE ( 'NONE', ( #1943 ), #10674, .T. ) ;
#3041 = CARTESIAN_POINT ( 'NONE',  ( -25.44486372867087454, 51.74373926088290432, -7.000000000000073719 ) ) ;
#3042 = CARTESIAN_POINT ( 'NONE',  ( -26.79131905728310059, 53.62708333237727487, -6.403925809002825709 ) ) ;
#3043 = DIRECTION ( 'NONE',  ( 0.000000000000000000, 0.000000000000000000, 1.000000000000000000 ) ) ;
#3044 = CARTESIAN_POINT ( 'NONE',  ( -0.6810597143197697489, -4.461075778259609770, -3.598441714920717516 ) ) ;
#3045 = CIRCLE ( 'NONE', #9239, 3.000000000000000000 ) ;
#3046 = ORIENTED_EDGE ( 'NONE', *, *, #9539, .T. ) ;
#3047 = CARTESIAN_POINT ( 'NONE',  ( -23.98076211353314235, 54.31249999808803608, -5.000000000000103029 ) ) ;
#3048 = FACE_OUTER_BOUND ( 'NONE', #2520, .T. ) ;
#3049 = ORIENTED_EDGE ( 'NONE', *, *, #2342, .F. ) ;
#3050 = ADVANCED_FACE ( 'NONE', ( #984 ), #2884, .F. ) ;
#3051 = CARTESIAN_POINT ( 'NONE',  ( -25.98076211353310683, 50.41874999904394627, -3.128098921329806714 ) ) ;
#3052 = VECTOR ( 'NONE', #2515, 999.9999999999998863 ) ;
#3053 = CARTESIAN_POINT ( 'NONE',  ( -25.98076211353310683, 50.24374999904394912, -3.128098921329806714 ) ) ;
#3054 = CARTESIAN_POINT ( 'NONE',  ( 17.60432978939287452, 17.35624782240900288, 11.07951759511215606 ) ) ;
#3055 = ORIENTED_EDGE ( 'NONE', *, *, #8179, .T. ) ;
#3056 = ORIENTED_EDGE ( 'NONE', *, *, #2967, .F. ) ;
#3057 = CARTESIAN_POINT ( 'NONE',  ( 4.101954839143059139, -2.368264730582948285, -3.681130640444269631 ) ) ;
#3058 = VERTEX_POINT ( 'NONE', #2666 ) ;
#3059 = DIRECTION ( 'NONE',  ( 0.000000000000000000, 0.000000000000000000, 1.000000000000000000 ) ) ;
#3060 = SURFACE_SIDE_STYLE ('',( #3891 ) ) ;
#3061 = VERTEX_POINT ( 'NONE', #9483 ) ;
#3062 = CARTESIAN_POINT ( 'NONE',  ( 19.48730207459018970, 19.05393922246432226, 11.95042449705224996 ) ) ;
#3063 = AXIS2_PLACEMENT_3D ( 'NONE', #2718, #924, #6874 ) ;
#3064 = CARTESIAN_POINT ( 'NONE',  ( 1.257172072275274388, -3.892973519170983110, -3.433252694550781303 ) ) ;
#3065 = CARTESIAN_POINT ( 'NONE',  ( 19.95752144772427528, 19.94857296576799754, 13.00425721518131184 ) ) ;
#3066 = CARTESIAN_POINT ( 'NONE',  ( -23.98076211353314235, 50.87083333142136610, -6.154700538379337615 ) ) ;
#3067 = CIRCLE ( 'NONE', #6078, 2.149999999999988809 ) ;
#3068 = CARTESIAN_POINT ( 'NONE',  ( 34.94281041931228771, 2.000000000000002220, -5.500000000000000000 ) ) ;
#3069 = DIRECTION ( 'NONE',  ( 1.000000000000000000, 6.098637220230963674E-17, 0.000000000000000000 ) ) ;
#3070 = ADVANCED_FACE ( 'NONE', ( #6041 ), #7882, .T. ) ;
#3071 = ORIENTED_EDGE ( 'NONE', *, *, #6203, .F. ) ;
#3072 = ORIENTED_EDGE ( 'NONE', *, *, #1458, .T. ) ;
#3073 = CARTESIAN_POINT ( 'NONE',  ( 17.91214753276079819, 17.12229137291643610, 13.05912755560225236 ) ) ;
#3074 = PLANE ( 'NONE',  #4366 ) ;
#3075 = CARTESIAN_POINT ( 'NONE',  ( -1.240299975428113101E-15, -4.647091401871173311, -3.572172305156514849 ) ) ;
#3076 = CARTESIAN_POINT ( 'NONE',  ( 5.076455387921339657, 24.47916666666667140, 2.500000000000000000 ) ) ;
#3077 = EDGE_CURVE ( 'NONE', #6815, #58, #6410, .T. ) ;
#3078 = CARTESIAN_POINT ( 'NONE',  ( 0.9693646802875628410, 32.52740819067395961, 12.58031658473306713 ) ) ;
#3079 = DIRECTION ( 'NONE',  ( 0.000000000000000000, 1.000000000000000000, 0.000000000000000000 ) ) ;
#3080 = UNCERTAINTY_MEASURE_WITH_UNIT (LENGTH_MEASURE( 1.000000000000000082E-05 ), #8638, 'distance_accuracy_value', 'NONE');
#3081 = VERTEX_POINT ( 'NONE', #5219 ) ;
#3082 = CARTESIAN_POINT ( 'NONE',  ( -25.98076211353311393, 55.18749999808803608, -7.000000000000072831 ) ) ;
#3083 = EDGE_CURVE ( 'NONE', #2599, #7325, #10373, .T. ) ;
#3084 = ORIENTED_EDGE ( 'NONE', *, *, #385, .T. ) ;
#3085 = CARTESIAN_POINT ( 'NONE',  ( -1.720978244806810498, 31.81455566112594013, 14.81030841526694175 ) ) ;
#3086 = CARTESIAN_POINT ( 'NONE',  ( -4.000000000000000000, 0.8730739991738342143, -3.223134629628428893 ) ) ;
#3087 = CARTESIAN_POINT ( 'NONE',  ( -23.98076211353314235, 52.15416666475469754, -3.845299461620867554 ) ) ;
#3088 = CARTESIAN_POINT ( 'NONE',  ( -2.500000000000005773, 29.99999999999999645, 13.96875000000000355 ) ) ;
#3089 = EDGE_CURVE ( 'NONE', #7474, #2294, #5274, .T. ) ;
#3090 = CARTESIAN_POINT ( 'NONE',  ( -26.51666049839535688, 51.10626073911683420, -7.000000000000074607 ) ) ;
#3091 = CARTESIAN_POINT ( 'NONE',  ( -26.79131905728310059, 51.35208333237728340, -6.403925809002825709 ) ) ;
#3092 = AXIS2_PLACEMENT_3D ( 'NONE', #8153, #5756, #9039 ) ;
#3093 = CARTESIAN_POINT ( 'NONE',  ( 2.000000000000008882, 3.464101615137749945, 0.000000000000000000 ) ) ;
#3094 = CARTESIAN_POINT ( 'NONE',  ( -3.540020015735593439, -2.810662092924100630, -3.602146406945814672 ) ) ;
#3095 = VERTEX_POINT ( 'NONE', #7827 ) ;
#3096 = CARTESIAN_POINT ( 'NONE',  ( 2.000000000000000000, 1.773042676681340524, -2.059984127722458425E-15 ) ) ;
#3097 = CARTESIAN_POINT ( 'NONE',  ( 2.650000000000097167, 30.00000000000000000, -2.500000000000000000 ) ) ;
#3098 = VECTOR ( 'NONE', #653, 1000.000000000000000 ) ;
#3099 = CARTESIAN_POINT ( 'NONE',  ( 0.000000000000000000, 0.000000000000000000, -9.500000000000000000 ) ) ;
#3100 = CARTESIAN_POINT ( 'NONE',  ( -25.98076211353310683, 54.79374999904395338, -6.871901078670399343 ) ) ;
#3101 = MECHANICAL_DESIGN_GEOMETRIC_PRESENTATION_REPRESENTATION (  '', ( #1681 ), #6638 ) ;
#3102 = CARTESIAN_POINT ( 'NONE',  ( 19.05040816462259556, 17.06282649731835122, 12.00984920396035172 ) ) ;
#3103 = CARTESIAN_POINT ( 'NONE',  ( -27.60187600103308370, 53.56874999904395196, -5.000000000000103029 ) ) ;
#3104 = CIRCLE ( 'NONE', #977, 2.000000000000000888 ) ;
#3105 = VERTEX_POINT ( 'NONE', #3602 ) ;
#3106 = CARTESIAN_POINT ( 'NONE',  ( 34.76670834929980458, 4.038474554490623980, 2.651503408690715435 ) ) ;
#3107 = ORIENTED_EDGE ( 'NONE', *, *, #1092, .T. ) ;
#3108 = ORIENTED_EDGE ( 'NONE', *, *, #720, .F. ) ;
#3109 = CARTESIAN_POINT ( 'NONE',  ( 29.50000000000000711, -9.999999999999998224, -12.50000000000000000 ) ) ;
#3110 = ORIENTED_EDGE ( 'NONE', *, *, #2623, .F. ) ;
#3111 = CARTESIAN_POINT ( 'NONE',  ( 2.500000000000000000, 0.000000000000000000, 0.000000000000000000 ) ) ;
#3112 = VECTOR ( 'NONE', #3435, 1000.000000000000000 ) ;
#3113 = ORIENTED_EDGE ( 'NONE', *, *, #6691, .F. ) ;
#3114 = VECTOR ( 'NONE', #8464, 1000.000000000000114 ) ;
#3115 = CARTESIAN_POINT ( 'NONE',  ( 19.17195227357822773, 19.49818538049391492, 10.95195840513741636 ) ) ;
#3116 = CARTESIAN_POINT ( 'NONE',  ( 0.2176891316980170965, -1.691919446222082346, -3.499999999999999112 ) ) ;
#3117 = CARTESIAN_POINT ( 'NONE',  ( 20.68923198420054987, 16.84571637733143490, 12.94889058896590583 ) ) ;
#3118 = CONICAL_SURFACE ( 'NONE', #6836, 5.560781378645573980, 1.221730476396046816 ) ;
#3119 = CARTESIAN_POINT ( 'NONE',  ( -25.98076211353311393, 53.43749999808803608, -2.690598923241634743 ) ) ;
#3120 = CARTESIAN_POINT ( 'NONE',  ( -25.98076211353310683, 53.52499999999986358, -3.000000000000132339 ) ) ;
#3121 = DIRECTION ( 'NONE',  ( -1.000000000000000000, -0.000000000000000000, -0.000000000000000000 ) ) ;
#3122 = VERTEX_POINT ( 'NONE', #202 ) ;
#3123 = ORIENTED_EDGE ( 'NONE', *, *, #8444, .T. ) ;
#3124 = CARTESIAN_POINT ( 'NONE',  ( 22.45328846257175925, 22.40877220821986171, 12.00579112326941988 ) ) ;
#3125 = AXIS2_PLACEMENT_3D ( 'NONE', #9351, #1747, #3410 ) ;
#3126 = DIRECTION ( 'NONE',  ( 0.000000000000000000, 0.000000000000000000, 1.000000000000000000 ) ) ;
#3127 = PLANE ( 'NONE',  #8017 ) ;
#3128 = CARTESIAN_POINT ( 'NONE',  ( -26.48810847200994090, 57.12842764990476496, -3.061534065193112220 ) ) ;
#3129 = CARTESIAN_POINT ( 'NONE',  ( -1.101703131577916883, 32.47259180932605460, 13.98656658473306713 ) ) ;
#3130 = CARTESIAN_POINT ( 'NONE',  ( -31.74999999999995737, 0.000000000000000000, 2.000000000000000888 ) ) ;
#3131 = ORIENTED_EDGE ( 'NONE', *, *, #8107, .F. ) ;
#3132 = DIRECTION ( 'NONE',  ( -0.000000000000000000, -0.000000000000000000, 1.000000000000000000 ) ) ;
#3133 = ORIENTED_EDGE ( 'NONE', *, *, #9054, .F. ) ;
#3134 = CARTESIAN_POINT ( 'NONE',  ( -3.472591809326048384, 31.51591669395100936, 14.88843341526694353 ) ) ;
#3135 = CARTESIAN_POINT ( 'NONE',  ( 0.000000000000000000, 0.000000000000000000, -25.03750572909317285 ) ) ;
#3136 = PRODUCT_RELATED_PRODUCT_CATEGORY ( 'part', '', ( #7066 ) ) ;
#3137 = DIRECTION ( 'NONE',  ( 1.000000000000000000, 6.098637220230964906E-17, 0.000000000000000000 ) ) ;
#3138 = DIRECTION ( 'NONE',  ( -1.000000000000000000, 0.000000000000000000, 0.000000000000000000 ) ) ;
#3139 = CARTESIAN_POINT ( 'NONE',  ( -31.74999999999995737, 0.000000000000000000, 2.500000000000000888 ) ) ;
#3140 = CARTESIAN_POINT ( 'NONE',  ( -25.98076211353311393, 51.64374999904395480, -3.128098921329806714 ) ) ;
#3141 = CARTESIAN_POINT ( 'NONE',  ( 2.887392608830372964, -2.020725942163647648, 3.499999999999999556 ) ) ;
#3142 = CYLINDRICAL_SURFACE ( 'NONE', #446, 3.000000000000000000 ) ;
#3143 = ORIENTED_EDGE ( 'NONE', *, *, #10749, .T. ) ;
#3144 = VECTOR ( 'NONE', #8753, 1000.000000000000000 ) ;
#3145 = COLOUR_RGB ( '', 0.08235294, 0.09019608, 0.10196078) ;
#3146 = LINE ( 'NONE', #4034, #1111 ) ;
#3147 = CARTESIAN_POINT ( 'NONE',  ( -25.98076211353311393, 49.49999999999986500, -5.000000000000103029 ) ) ;
#3148 = EDGE_CURVE ( 'NONE', #8043, #9486, #8725, .T. ) ;
#3149 = ADVANCED_FACE ( 'NONE', ( #9544 ), #9507, .T. ) ;
#3150 = LINE ( 'NONE', #532, #8420 ) ;
#3151 = CARTESIAN_POINT ( 'NONE',  ( -27.60187600103308370, 51.46874999904395054, -5.000000000000103029 ) ) ;
#3152 = CONICAL_SURFACE ( 'NONE', #5994, 2.500000000000000888, 0.9599310885968785900 ) ;
#3153 = CARTESIAN_POINT ( 'NONE',  ( 22.45328846257175925, 22.40877220821986171, 12.00579112326941988 ) ) ;
#3154 = CARTESIAN_POINT ( 'NONE',  ( -24.98076211353313170, 50.08333333333319359, -3.267949192431250705 ) ) ;
#3155 = EDGE_LOOP ( 'NONE', ( #1792, #9989 ) ) ;
#3156 = CARTESIAN_POINT ( 'NONE',  ( 3.061158938895440773, -2.351840044243218131, -2.926493552095763118 ) ) ;
#3157 = ORIENTED_EDGE ( 'NONE', *, *, #5699, .T. ) ;
#3158 = ORIENTED_EDGE ( 'NONE', *, *, #500, .F. ) ;
#3159 = DIRECTION ( 'NONE',  ( 0.000000000000000000, 0.000000000000000000, 1.000000000000000000 ) ) ;
#3160 = VERTEX_POINT ( 'NONE', #5497 ) ;
#3161 = EDGE_CURVE ( 'NONE', #7127, #6258, #8042, .T. ) ;
#3162 = CARTESIAN_POINT ( 'NONE',  ( 24.49999999999999289, -3.999999999999986233, -4.999999999999992006 ) ) ;
#3163 = ORIENTED_EDGE ( 'NONE', *, *, #7859, .T. ) ;
#3164 = STYLED_ITEM ( 'NONE', ( #8028 ), #1777 ) ;
#3165 = CARTESIAN_POINT ( 'NONE',  ( 23.11946528304491011, 21.60344811844516499, 11.00732503135595941 ) ) ;
#3166 = DIRECTION ( 'NONE',  ( 1.000000000000000000, 0.000000000000000000, 0.000000000000000000 ) ) ;
#3167 = CARTESIAN_POINT ( 'NONE',  ( 4.141042297810615835, -2.227970268150433863, -3.687027686973623819 ) ) ;
#3168 = EDGE_CURVE ( 'NONE', #9486, #7127, #4898, .T. ) ;
#3169 = CARTESIAN_POINT ( 'NONE',  ( 19.76265562249496099, 16.28401831655332543, 11.95127577209155234 ) ) ;
#3170 = CARTESIAN_POINT ( 'NONE',  ( -26.98076211353309972, 50.57916666475469469, -3.267949192431252037 ) ) ;
#3171 = CARTESIAN_POINT ( 'NONE',  ( 3.999999999999999112, -0.3979232138631231819, -5.929230630780099908E-17 ) ) ;
#3172 = CARTESIAN_POINT ( 'NONE',  ( -25.98076211353311038, 59.49999999999985789, -5.000000000000102141 ) ) ;
#3173 = VERTEX_POINT ( 'NONE', #8198 ) ;
#3174 = CARTESIAN_POINT ( 'NONE',  ( 1.449747468305833120, 33.50000000000000000, 13.57812500000000178 ) ) ;
#3175 = ORIENTED_EDGE ( 'NONE', *, *, #772, .T. ) ;
#3176 = CARTESIAN_POINT ( 'NONE',  ( 23.68215991433358525, 19.03072201379386641, 12.94889058896590583 ) ) ;
#3177 = EDGE_CURVE ( 'NONE', #9108, #3195, #1373, .T. ) ;
#3178 = DIRECTION ( 'NONE',  ( 0.000000000000000000, 1.000000000000000000, 0.000000000000000000 ) ) ;
#3179 =( BOUNDED_CURVE ( )  B_SPLINE_CURVE ( 1, ( #7134, #10529 ),
 .UNSPECIFIED., .F., .F. ) 
 B_SPLINE_CURVE_WITH_KNOTS ( ( 2, 2 ),
 ( 0.000000000000000000, 1.000000000000000000 ),
 .UNSPECIFIED. ) 
 CURVE ( )  GEOMETRIC_REPRESENTATION_ITEM ( )  RATIONAL_B_SPLINE_CURVE ( ( 0.9343183815700366601, 0.9343183815700366601 ) ) 
 REPRESENTATION_ITEM ( '' )  );
#3180 = CARTESIAN_POINT ( 'NONE',  ( 34.69563600136375214, 4.609751841799207384, 2.519143709543159471 ) ) ;
#3181 = CARTESIAN_POINT ( 'NONE',  ( -31.74999999999995737, 0.000000000000000000, 4.250000000000000000 ) ) ;
#3182 = CARTESIAN_POINT ( 'NONE',  ( 0.9693646802875628410, 32.52740819067395961, 13.83031658473306535 ) ) ;
#3183 = CYLINDRICAL_SURFACE ( 'NONE', #7746, 0.4999999999999883982 ) ;
#3184 = VERTEX_POINT ( 'NONE', #5703 ) ;
#3185 = CARTESIAN_POINT ( 'NONE',  ( -25.98076211353311393, 49.49999999999986500, -5.000000000000103029 ) ) ;
#3186 = ORIENTED_EDGE ( 'NONE', *, *, #3436, .F. ) ;
#3187 = CARTESIAN_POINT ( 'NONE',  ( 1.814555661125939467, 31.72097824480680828, 14.49780841526694175 ) ) ;
#3188 = LINE ( 'NONE', #465, #6642 ) ;
#3189 = DIRECTION ( 'NONE',  ( 0.6587175828649983744, -0.7523902883640206651, 4.024558464266192459E-16 ) ) ;
#3190 = DIRECTION ( 'NONE',  ( 0.000000000000000000, 0.000000000000000000, 1.000000000000000000 ) ) ;
#3191 = DIRECTION ( 'NONE',  ( 1.000000000000000000, 0.000000000000000000, 0.000000000000000000 ) ) ;
#3192 = CARTESIAN_POINT ( 'NONE',  ( -26.79131905728310059, 49.95208333237728482, -6.403925809002825709 ) ) ;
#3193 = CARTESIAN_POINT ( 'NONE',  ( 3.170625919164821394, -0.6808742863894992059, 3.500000000000000000 ) ) ;
#3194 = CARTESIAN_POINT ( 'NONE',  ( 2.682243648011666703, 3.070208061305304881, -0.04852650426601266831 ) ) ;
#3195 = VERTEX_POINT ( 'NONE', #4610 ) ;
#3196 = CARTESIAN_POINT ( 'NONE',  ( -1.449747468305836229, 33.50000000000000000, 14.98437500000000533 ) ) ;
#3197 = CARTESIAN_POINT ( 'NONE',  ( 11.99999999999999645, 0.000000000000000000, 0.000000000000000000 ) ) ;
#3198 = EDGE_CURVE ( 'NONE', #4891, #7578, #10742, .T. ) ;
#3199 = CARTESIAN_POINT ( 'NONE',  ( -25.17020516978313083, 50.01041666571061484, -6.403925809002825709 ) ) ;
#3200 = CARTESIAN_POINT ( 'NONE',  ( -26.79131905728310059, 51.58541666571061768, -3.596074190997381237 ) ) ;
#3201 = B_SPLINE_CURVE_WITH_KNOTS ( 'NONE', 3,
 ( #5702, #1426, #3193, #9975, #8094, #3141 ),
 .UNSPECIFIED., .F., .F.,
 ( 4, 2, 4 ),
 ( 0.01103649464086231546, 0.01205977283736816077, 0.01308305103387400609 ),
 .UNSPECIFIED. ) ;
#3202 = CARTESIAN_POINT ( 'NONE',  ( 23.17052989764754756, 21.62756661655841839, 12.00579112326981246 ) ) ;
#3203 = CARTESIAN_POINT ( 'NONE',  ( -26.98076211353309972, 50.43333333333319501, -6.732050807568954909 ) ) ;
#3204 = ORIENTED_EDGE ( 'NONE', *, *, #5400, .F. ) ;
#3205 = ADVANCED_FACE ( 'NONE', ( #8150 ), #3142, .F. ) ;
#3206 = CARTESIAN_POINT ( 'NONE',  ( -25.17020516978313083, 55.37708333237728198, -3.596074190997380349 ) ) ;
#3207 = ORIENTED_EDGE ( 'NONE', *, *, #793, .T. ) ;
#3208 = ORIENTED_EDGE ( 'NONE', *, *, #1805, .F. ) ;
#3209 = PLANE ( 'NONE',  #8428 ) ;
#3210 = EDGE_LOOP ( 'NONE', ( #4076, #3440, #9214, #10338, #5343, #4622, #6043, #2586 ) ) ;
#3211 = EDGE_CURVE ( 'NONE', #3226, #4884, #4545, .T. ) ;
#3212 = DIRECTION ( 'NONE',  ( 0.000000000000000000, 0.000000000000000000, 1.000000000000000000 ) ) ;
#3213 =( NAMED_UNIT ( * ) PLANE_ANGLE_UNIT ( ) SI_UNIT ( $, .RADIAN. ) );
#3214 = VECTOR ( 'NONE', #188, 1000.000000000000000 ) ;
#3215 = ORIENTED_EDGE ( 'NONE', *, *, #7423, .F. ) ;
#3216 = CARTESIAN_POINT ( 'NONE',  ( 16.11564427137601285, 18.83410319690818824, 12.22072830420661660 ) ) ;
#3217 =( NAMED_UNIT ( * ) PLANE_ANGLE_UNIT ( ) SI_UNIT ( $, .RADIAN. ) );
#3218 = DIRECTION ( 'NONE',  ( 4.312387734421999162E-17, -0.7071067811865487940, 0.7071067811865463515 ) ) ;
#3219 = CARTESIAN_POINT ( 'NONE',  ( -4.154094228333736538, -2.398367420967545627, -3.721909803043222276 ) ) ;
#3220 = CARTESIAN_POINT ( 'NONE',  ( 17.43584335925693196, 16.24128823292743817, 13.04062965360331106 ) ) ;
#3221 = EDGE_CURVE ( 'NONE', #4005, #2047, #526, .T. ) ;
#3222 = CARTESIAN_POINT ( 'NONE',  ( -23.98076211353314235, 52.15416666475470464, -3.845299461620867554 ) ) ;
#3223 = DIRECTION ( 'NONE',  ( 0.000000000000000000, -0.8660254037844431485, -0.4999999999999921729 ) ) ;
#3224 = CARTESIAN_POINT ( 'NONE',  ( 34.99999999999987210, -9.999999999999998224, -10.50000000000001243 ) ) ;
#3225 = PRODUCT_DEFINITION_CONTEXT ( 'detailed design', #8765, 'design' ) ;
#3226 = VERTEX_POINT ( 'NONE', #3972 ) ;
#3227 = CARTESIAN_POINT ( 'NONE',  ( 3.500000000000007994, 29.93383077435482420, 15.59155841526693997 ) ) ;
#3228 = CONICAL_SURFACE ( 'NONE', #6068, 1.610000000000000098, 0.7853981633974741472 ) ;
#3229 = EDGE_LOOP ( 'NONE', ( #6223, #10215, #2667, #9993 ) ) ;
#3230 = APPLICATION_CONTEXT ( 'automotive_design' ) ;
#3231 = EDGE_CURVE ( 'NONE', #8338, #4274, #5041, .T. ) ;
#3232 = ADVANCED_FACE ( 'NONE', ( #2940 ), #2155, .T. ) ;
#3233 = CARTESIAN_POINT ( 'NONE',  ( 23.37401553338360571, 20.56828919810574519, 13.00425721518307753 ) ) ;
#3234 = CARTESIAN_POINT ( 'NONE',  ( -30.75045812061784289, 13.49999999999941913, -2.500000000000000000 ) ) ;
#3235 = DIRECTION ( 'NONE',  ( -1.000000000000000000, -6.098637220230963674E-17, -1.156482317317871478E-16 ) ) ;
#3236 = AXIS2_PLACEMENT_3D ( 'NONE', #8985, #2264, #5658 ) ;
#3237 = CARTESIAN_POINT ( 'NONE',  ( 34.99999999999999289, -3.999999999999993339, 7.850000000000016520 ) ) ;
#3238 = CARTESIAN_POINT ( 'NONE',  ( 3.472591809326047052, 31.51591669395100936, 13.67406658473306535 ) ) ;
#3239 = FACE_OUTER_BOUND ( 'NONE', #2406, .T. ) ;
#3240 = FACE_BOUND ( 'NONE', #8928, .T. ) ;
#3241 = CARTESIAN_POINT ( 'NONE',  ( -25.98076211353310683, 55.53749999808803040, -3.000000000000132339 ) ) ;
#3242 = ORIENTED_EDGE ( 'NONE', *, *, #9626, .F. ) ;
#3243 = ORIENTED_EDGE ( 'NONE', *, *, #5785, .F. ) ;
#3244 = CARTESIAN_POINT ( 'NONE',  ( -25.98076211353324894, 14.99999999999984190, -2.500000000000000000 ) ) ;
#3245 = CARTESIAN_POINT ( 'NONE',  ( -6.259644161404860030E-16, -4.618802153517027165, -5.000000000000000000 ) ) ;
#3246 = CARTESIAN_POINT ( 'NONE',  ( -25.98076211353311393, 49.49999999999986500, -3.000000000000131894 ) ) ;
#3247 = DIRECTION ( 'NONE',  ( -1.000000000000000000, 0.000000000000000000, 0.000000000000000000 ) ) ;
#3248 = ADVANCED_FACE ( 'NONE', ( #3817 ), #8509, .F. ) ;
#3249 = DIRECTION ( 'NONE',  ( 0.000000000000000000, 0.000000000000000000, -1.000000000000000000 ) ) ;
#3250 = CARTESIAN_POINT ( 'NONE',  ( -25.98076211353311393, 55.66874999904395338, -6.871901078670400231 ) ) ;
#3251 = DIRECTION ( 'NONE',  ( 0.000000000000000000, 0.000000000000000000, -1.000000000000000000 ) ) ;
#3252 = CARTESIAN_POINT ( 'NONE',  ( -25.98076211353324894, 14.99999999999984190, 2.500000000000000000 ) ) ;
#3253 = ORIENTED_EDGE ( 'NONE', *, *, #10957, .T. ) ;
#3254 = CARTESIAN_POINT ( 'NONE',  ( -1.449747468305836229, 33.50000000000000000, 13.73437500000000888 ) ) ;
#3255 = CARTESIAN_POINT ( 'NONE',  ( -2.500000000000005773, 29.99999999999999645, 13.96875000000000355 ) ) ;
#3256 = CARTESIAN_POINT ( 'NONE',  ( -26.98076211353309972, 53.93333333333319501, -6.732050807568954909 ) ) ;
#3257 = CARTESIAN_POINT ( 'NONE',  ( -27.60187600103308370, 51.64374999904394770, -5.000000000000103029 ) ) ;
#3258 = CARTESIAN_POINT ( 'NONE',  ( -24.35964822603314772, 53.97708333237729050, -5.935950539335252074 ) ) ;
#3259 = CARTESIAN_POINT ( 'NONE',  ( 18.62184541094303114, 16.98042197548449295, 12.02177981800743112 ) ) ;
#3260 = CARTESIAN_POINT ( 'NONE',  ( -26.98076211353309972, 52.06666666666653498, -3.267949192431252037 ) ) ;
#3261 = ORIENTED_EDGE ( 'NONE', *, *, #7499, .F. ) ;
#3262 = ORIENTED_EDGE ( 'NONE', *, *, #7335, .F. ) ;
#3263 = ORIENTED_EDGE ( 'NONE', *, *, #2830, .T. ) ;
#3264 = PLANE ( 'NONE',  #1488 ) ;
#3265 = ORIENTED_EDGE ( 'NONE', *, *, #8857, .T. ) ;
#3266 = DIRECTION ( 'NONE',  ( 0.000000000000000000, 0.000000000000000000, 1.000000000000000000 ) ) ;
#3267 = DIRECTION ( 'NONE',  ( 0.000000000000000000, 0.000000000000000000, 1.000000000000000000 ) ) ;
#3268 = ORIENTED_EDGE ( 'NONE', *, *, #1600, .F. ) ;
#3269 = CARTESIAN_POINT ( 'NONE',  ( 22.10027471249113162, 22.50626116107413921, 11.00732503135576401 ) ) ;
#3270 =( LENGTH_UNIT ( ) NAMED_UNIT ( * ) SI_UNIT ( .MILLI., .METRE. ) );
#3271 = STYLED_ITEM ( 'NONE', ( #2814 ), #8973 ) ;
#3272 = PRESENTATION_STYLE_ASSIGNMENT (( #10416 ) ) ;
#3273 = CLOSED_SHELL ( 'NONE', ( #8289, #9821, #360, #167, #2502, #545, #6210, #6896, #10094, #7838, #5815, #589, #1948, #4252, #33, #5604, #5660, #4014, #8170, #5864, #10955, #9080, #3832, #49, #3205, #6975, #10069, #9446, #7435, #2612, #1520, #1865, #8528, #3425, #2070, #6690, #4370, #3050, #7009, #7711, #8496, #6925, #4383 ) ) ;
#3274 = VECTOR ( 'NONE', #8714, 1000.000000000000000 ) ;
#3275 = CARTESIAN_POINT ( 'NONE',  ( -24.35964822603314772, 50.53541666571060631, -4.064049460664953983 ) ) ;
#3276 = CARTESIAN_POINT ( 'NONE',  ( 24.08125446323534291, 19.61299372598402613, 12.94889058896590761 ) ) ;
#3277 = FILL_AREA_STYLE_COLOUR ( '', #3876 ) ;
#3278 = CARTESIAN_POINT ( 'NONE',  ( -24.98076211353313170, 54.19583333142136894, -3.267949192431250705 ) ) ;
#3279 = CIRCLE ( 'NONE', #3818, 2.055000000000000160 ) ;
#3280 = DIRECTION ( 'NONE',  ( 0.000000000000000000, -0.000000000000000000, -1.000000000000000000 ) ) ;
#3281 = EDGE_LOOP ( 'NONE', ( #8547, #2045, #3514, #2363 ) ) ;
#3282 = DIRECTION ( 'NONE',  ( -0.8191520442889902442, 0.000000000000000000, -0.5735764363510482688 ) ) ;
#3283 = VERTEX_POINT ( 'NONE', #10751 ) ;
#3284 = AXIS2_PLACEMENT_3D ( 'NONE', #6497, #1452, #3949 ) ;
#3285 = CARTESIAN_POINT ( 'NONE',  ( 3.903127820947815962E-15, 26.49999999999999289, 14.28125000000000355 ) ) ;
#3286 = AXIS2_PLACEMENT_3D ( 'NONE', #186, #7130, #1920 ) ;
#3287 = CONICAL_SURFACE ( 'NONE', #611, 3.499999999999999556, 1.047197551196603849 ) ;
#3288 = ORIENTED_EDGE ( 'NONE', *, *, #573, .F. ) ;
#3289 = CARTESIAN_POINT ( 'NONE',  ( 21.07893270796819962, 17.11679519544646411, 12.94889058896590583 ) ) ;
#3290 = ADVANCED_FACE ( 'NONE', ( #2312 ), #10809, .F. ) ;
#3291 = EDGE_CURVE ( 'NONE', #7662, #6545, #9864, .T. ) ;
#3292 = VECTOR ( 'NONE', #347, 1000.000000000000000 ) ;
#3293 = DIRECTION ( 'NONE',  ( 1.000000000000000000, 0.000000000000000000, 0.000000000000000000 ) ) ;
#3294 = CARTESIAN_POINT ( 'NONE',  ( -4.379688272585405606, 36.08837668307224789, -2.499999999999998668 ) ) ;
#3296 = DIRECTION ( 'NONE',  ( -1.000000000000000000, -0.000000000000000000, -0.000000000000000000 ) ) ;
#3295 = CONICAL_SURFACE ( 'NONE', #8254, 3.500000000000591971, 0.7853981633974560506 ) ;
#3297 = CARTESIAN_POINT ( 'NONE',  ( -3.527408190673960053, 31.38357824266065066, 15.39281658473306358 ) ) ;
#3298 = CARTESIAN_POINT ( 'NONE',  ( -24.98076211353313170, 51.39583333142136468, -3.267949192431250705 ) ) ;
#3299 = ORIENTED_EDGE ( 'NONE', *, *, #9322, .F. ) ;
#3300 = CARTESIAN_POINT ( 'NONE',  ( 3.200000000000000178, 0.3418418480469889165, 3.499999999999999556 ) ) ;
#3301 = ORIENTED_EDGE ( 'NONE', *, *, #8526, .T. ) ;
#3302 = ORIENTED_EDGE ( 'NONE', *, *, #3148, .T. ) ;
#3303 = DIRECTION ( 'NONE',  ( 1.000000000000000000, 0.000000000000000000, 0.000000000000000000 ) ) ;
#3304 = CIRCLE ( 'NONE', #6318, 2.100000000000000089 ) ;
#3305 = CARTESIAN_POINT ( 'NONE',  ( -4.197312064133472020, -0.8182229787990021874, -3.502518405183886685 ) ) ;
#3306 = CARTESIAN_POINT ( 'NONE',  ( 19.85760542366876535, 20.31250532737884384, 12.00579112326941988 ) ) ;
#3307 = CARTESIAN_POINT ( 'NONE',  ( 1.035533905932737975, 32.50000000000000711, 13.57812500000000533 ) ) ;
#3308 = CYLINDRICAL_SURFACE ( 'NONE', #1615, 1.500000000000001332 ) ;
#3309 = CARTESIAN_POINT ( 'NONE',  ( -25.17020516978313083, 51.23541666571061626, -6.403925809002825709 ) ) ;
#3310 = DIRECTION ( 'NONE',  ( -0.000000000000000000, 1.000000000000000000, -0.000000000000000000 ) ) ;
#3311 = CARTESIAN_POINT ( 'NONE',  ( 3.349226789952652439, 2.685125164760731487, -0.2236248678334773199 ) ) ;
#3312 = VERTEX_POINT ( 'NONE', #10093 ) ;
#3313 = CIRCLE ( 'NONE', #438, 1.650000000000000355 ) ;
#3314 = CARTESIAN_POINT ( 'NONE',  ( 29.49999999999999289, -9.999999999999998224, 15.50000000000000533 ) ) ;
#3315 = LINE ( 'NONE', #1706, #4601 ) ;
#3316 = CARTESIAN_POINT ( 'NONE',  ( -25.17020516978313083, 52.81041666571061199, -6.403925809002825709 ) ) ;
#3317 = EDGE_CURVE ( 'NONE', #10481, #5606, #806, .T. ) ;
#3318 = CARTESIAN_POINT ( 'NONE',  ( -26.79131905728310059, 54.85208333237729050, -6.403925809002825709 ) ) ;
#3319 = CARTESIAN_POINT ( 'NONE',  ( 29.50000000000000711, 2.000000000000001776, -10.49999999999999822 ) ) ;
#3320 = VECTOR ( 'NONE', #6303, 1000.000000000000114 ) ;
#3321 = CARTESIAN_POINT ( 'NONE',  ( -27.98076211353308551, 52.64999999999986358, -5.000000000000103029 ) ) ;
#3322 = ORIENTED_EDGE ( 'NONE', *, *, #6483, .F. ) ;
#3323 = ORIENTED_EDGE ( 'NONE', *, *, #3198, .T. ) ;
#3324 = VERTEX_POINT ( 'NONE', #5866 ) ;
#3325 = CARTESIAN_POINT ( 'NONE',  ( 5.000000000000002665, 0.000000000000000000, -2.700000000000001066 ) ) ;
#3326 = VERTEX_POINT ( 'NONE', #26 ) ;
#3327 = CARTESIAN_POINT ( 'NONE',  ( -25.98076211353311393, 59.49999999999985789, -3.000000000000131894 ) ) ;
#3328 = FILL_AREA_STYLE_COLOUR ( '', #476 ) ;
#3329 = VERTEX_POINT ( 'NONE', #9303 ) ;
#3331 = CARTESIAN_POINT ( 'NONE',  ( 18.27511531525127353, 17.01097670698189290, 12.03680973694848966 ) ) ;
#3330 = VECTOR ( 'NONE', #5289, 1000.000000000000000 ) ;
#3332 = VECTOR ( 'NONE', #7557, 1000.000000000000000 ) ;
#3333 =( NAMED_UNIT ( * ) PLANE_ANGLE_UNIT ( ) SI_UNIT ( $, .RADIAN. ) );
#3334 = DIRECTION ( 'NONE',  ( -4.312387734421975126E-17, 0.7071067811865451302, 0.7071067811865500152 ) ) ;
#3335 = FACE_OUTER_BOUND ( 'NONE', #5989, .T. ) ;
#3336 = CARTESIAN_POINT ( 'NONE',  ( 21.85833415550051484, 17.65895283167741425, 12.94889058896590583 ) ) ;
#3337 = SURFACE_STYLE_USAGE ( .BOTH. , #5531 ) ;
#3338 = CARTESIAN_POINT ( 'NONE',  ( -23.98076211353314235, 55.65416666475469754, -3.845299461620867554 ) ) ;
#3339 = CIRCLE ( 'NONE', #851, 3.249999999999998668 ) ;
#3340 =( GEOMETRIC_REPRESENTATION_CONTEXT ( 3 ) GLOBAL_UNCERTAINTY_ASSIGNED_CONTEXT ( ( #3649 ) ) GLOBAL_UNIT_ASSIGNED_CONTEXT ( ( #3017, #5006, #10832 ) ) REPRESENTATION_CONTEXT ( 'NONE', 'WORKASPACE' ) );
#3341 = CARTESIAN_POINT ( 'NONE',  ( -24.98076211353313170, 53.58333333333320070, -3.267949192431250705 ) ) ;
#3342 = ORIENTED_EDGE ( 'NONE', *, *, #7314, .F. ) ;
#3343 = CARTESIAN_POINT ( 'NONE',  ( 0.000000000000000000, 0.000000000000000000, 3.469446951953614189E-15 ) ) ;
#3344 = ORIENTED_EDGE ( 'NONE', *, *, #10382, .F. ) ;
#3345 = AXIS2_PLACEMENT_3D ( 'NONE', #5480, #4436, #1613 ) ;
#3346 = CARTESIAN_POINT ( 'NONE',  ( -3.500000000000005329, 30.06616922564516869, 16.21655841526694175 ) ) ;
#3347 = ORIENTED_EDGE ( 'NONE', *, *, #7703, .T. ) ;
#3348 = EDGE_CURVE ( 'NONE', #58, #6815, #2055, .T. ) ;
#3349 = CARTESIAN_POINT ( 'NONE',  ( 17.82816014985957054, 16.05830732944317418, 13.01541525850460168 ) ) ;
#3350 = CARTESIAN_POINT ( 'NONE',  ( 0.000000000000000000, 0.000000000000000000, -0.2800830152838844622 ) ) ;
#3351 = CONICAL_SURFACE ( 'NONE', #1036, 1.649999999999998579, 1.029744258676653423 ) ;
#3352 = DIRECTION ( 'NONE',  ( -1.000000000000000000, 0.000000000000000000, 0.000000000000000000 ) ) ;
#3353 = CARTESIAN_POINT ( 'NONE',  ( 5.791420021395468964, -3.168237633705329831E-17, 0.000000000000000000 ) ) ;
#3354 = CARTESIAN_POINT ( 'NONE',  ( -2.500000000000004441, 28.96446609406725159, 14.04687500000000355 ) ) ;
#3355 = CARTESIAN_POINT ( 'NONE',  ( -5.384454397937118664, 6.702023979852544604E-16, -5.000000000000000000 ) ) ;
#3356 = CARTESIAN_POINT ( 'NONE',  ( 25.58039891549807976, 2.000000000000002665, 2.500000000000000444 ) ) ;
#3357 = CARTESIAN_POINT ( 'NONE',  ( 4.197393957002303999, 7.772902908466098641E-14, -3.503767560748929810 ) ) ;
#3358 = EDGE_CURVE ( 'NONE', #3095, #1804, #2402, .T. ) ;
#3359 = ORIENTED_EDGE ( 'NONE', *, *, #1117, .T. ) ;
#3360 = ORIENTED_EDGE ( 'NONE', *, *, #3422, .T. ) ;
#3361 = ADVANCED_FACE ( 'NONE', ( #10200 ), #1205, .F. ) ;
#3362 = DIRECTION ( 'NONE',  ( -0.000000000000000000, 0.000000000000000000, -1.000000000000000000 ) ) ;
#3363 = DIRECTION ( 'NONE',  ( 1.000000000000000000, -0.000000000000000000, 1.156482317317871478E-16 ) ) ;
#3364 = CARTESIAN_POINT ( 'NONE',  ( 22.45328846257175925, 22.40877220821986171, 12.00579112326941988 ) ) ;
#3365 = CARTESIAN_POINT ( 'NONE',  ( -1.767766952966375094, 31.76776695296636888, 16.31250000000000355 ) ) ;
#3366 = CARTESIAN_POINT ( 'NONE',  ( -25.98076211353311393, 49.49999999999986500, -3.000000000000131894 ) ) ;
#3367 = CARTESIAN_POINT ( 'NONE',  ( -27.60187600103308014, 53.62708333237728908, -4.064049460664955760 ) ) ;
#3368 = LINE ( 'NONE', #9471, #4589 ) ;
#3369 = CARTESIAN_POINT ( 'NONE',  ( 0.000000000000000000, 3.031088913245510774, -1.750000000000042411 ) ) ;
#3370 = CARTESIAN_POINT ( 'NONE',  ( -25.98076211353311038, 61.49999999999985789, -5.000000000000102141 ) ) ;
#3371 = EDGE_CURVE ( 'NONE', #3819, #6902, #7738, .T. ) ;
#3372 = ORIENTED_EDGE ( 'NONE', *, *, #2762, .F. ) ;
#3373 = CARTESIAN_POINT ( 'NONE',  ( 24.30992024302470256, 5.833333333333333925, 2.500000000000000000 ) ) ;
#3374 = CARTESIAN_POINT ( 'NONE',  ( -26.98076211353309972, 54.16666666666652930, -3.267949192431252037 ) ) ;
#3375 = ADVANCED_FACE ( 'NONE', ( #4985 ), #7592, .T. ) ;
#3376 = CARTESIAN_POINT ( 'NONE',  ( -25.98076211353310683, 54.61874999904394912, -3.128098921329806714 ) ) ;
#3377 = CARTESIAN_POINT ( 'NONE',  ( 2.000000000000000000, -1.773042676681341856, 2.276824562219559311E-15 ) ) ;
#3378 = DIRECTION ( 'NONE',  ( -1.000000000000000000, -0.000000000000000000, -0.000000000000000000 ) ) ;
#3379 = CARTESIAN_POINT ( 'NONE',  ( -23.98076211353314235, 53.69999999999986784, -5.000000000000103029 ) ) ;
#3380 = ORIENTED_EDGE ( 'NONE', *, *, #9822, .T. ) ;
#3381 = VERTEX_POINT ( 'NONE', #1532 ) ;
#3383 = ORIENTED_EDGE ( 'NONE', *, *, #8476, .F. ) ;
#3382 = ADVANCED_FACE ( 'NONE', ( #5919 ), #3295, .T. ) ;
#3384 = CARTESIAN_POINT ( 'NONE',  ( 25.78460820925620922, 50.00384911698630930, -2.500000000000000000 ) ) ;
#3385 = VERTEX_POINT ( 'NONE', #2482 ) ;
#3386 = CARTESIAN_POINT ( 'NONE',  ( 29.49999999999999289, 2.000000000000001776, 5.500000000000000000 ) ) ;
#3387 = DIRECTION ( 'NONE',  ( -0.9999999999999998890, 2.775557561562891351E-17, -1.387778780781445676E-17 ) ) ;
#3388 = ORIENTED_EDGE ( 'NONE', *, *, #4917, .F. ) ;
#3389 = CARTESIAN_POINT ( 'NONE',  ( 21.48473758187327931, 18.75023854587115935, 11.00732503135576401 ) ) ;
#3390 = DIRECTION ( 'NONE',  ( 4.312387734421982522E-17, -0.7071067811865462405, 0.7071067811865487940 ) ) ;
#3391 = FACE_OUTER_BOUND ( 'NONE', #5056, .T. ) ;
#3392 = CARTESIAN_POINT ( 'NONE',  ( 20.65761543282678758, 16.89116807672653664, 11.95042449705224819 ) ) ;
#3393 = CARTESIAN_POINT ( 'NONE',  ( -25.98076211353311038, 59.49999999999985789, -9.000000000000701661 ) ) ;
#3394 = CARTESIAN_POINT ( 'NONE',  ( -26.79131905728310059, 51.06041666571061199, -3.596074190997381237 ) ) ;
#3395 = AXIS2_PLACEMENT_3D ( 'NONE', #6191, #3538, #1977 ) ;
#3396 = PLANE ( 'NONE',  #9824 ) ;
#3397 = EDGE_LOOP ( 'NONE', ( #370, #8416, #9099, #3517, #3439 ) ) ;
#3398 = DIRECTION ( 'NONE',  ( -1.000000000000000000, -0.000000000000000000, -0.000000000000000000 ) ) ;
#3399 = ORIENTED_EDGE ( 'NONE', *, *, #1796, .F. ) ;
#3400 = CARTESIAN_POINT ( 'NONE',  ( -2.474873734152920335, 32.47487373415291501, 15.06250000000000355 ) ) ;
#3401 = ORIENTED_EDGE ( 'NONE', *, *, #7038, .F. ) ;
#3402 = CARTESIAN_POINT ( 'NONE',  ( 23.26157621925297647, 18.63507786824203549, 12.94889058896600353 ) ) ;
#3403 = VECTOR ( 'NONE', #10846, 1000.000000000000000 ) ;
#3404 = EDGE_CURVE ( 'NONE', #1738, #2370, #4004, .T. ) ;
#3405 = DIRECTION ( 'NONE',  ( 1.000000000000000000, 0.000000000000000000, 0.000000000000000000 ) ) ;
#3406 = CARTESIAN_POINT ( 'NONE',  ( 19.55162244606592381, 17.33808635661342024, 12.00579012602852735 ) ) ;
#3407 = CARTESIAN_POINT ( 'NONE',  ( -25.17020516978313083, 52.40208333237728766, -3.596074190997380349 ) ) ;
#3408 = EDGE_CURVE ( 'NONE', #10201, #1840, #8359, .T. ) ;
#3409 = CARTESIAN_POINT ( 'NONE',  ( 2.500000000000007550, 31.03553390593274486, 14.67187500000000178 ) ) ;
#3410 = DIRECTION ( 'NONE',  ( 0.000000000000000000, 0.000000000000000000, -1.000000000000000000 ) ) ;
#3411 = CARTESIAN_POINT ( 'NONE',  ( 0.000000000000000000, -3.031088913245509886, 1.750000000000043077 ) ) ;
#3412 = CARTESIAN_POINT ( 'NONE',  ( 24.49999999999999289, 0.5000000000000132117, -4.999999999999992006 ) ) ;
#3413 = EDGE_LOOP ( 'NONE', ( #6855, #1806 ) ) ;
#3414 = VERTEX_POINT ( 'NONE', #4139 ) ;
#3415 = CARTESIAN_POINT ( 'NONE',  ( 0.1388410611046201060, 3.710337782248057437, 0.5735064479039569951 ) ) ;
#3416 = DIRECTION ( 'NONE',  ( 1.000000000000000000, 6.098637220230963674E-17, -0.000000000000000000 ) ) ;
#3417 = PRODUCT ( 'caliper arm right', 'caliper arm right', '', ( #7210 ) ) ;
#3418 = CARTESIAN_POINT ( 'NONE',  ( 20.73695268571362504, 18.16262921024512167, 12.00579112326941988 ) ) ;
#3419 = VECTOR ( 'NONE', #8149, 1000.000000000000000 ) ;
#3420 = PRODUCT_DEFINITION ( 'UNKNOWN', '', #7574, #3225 ) ;
#3421 = CARTESIAN_POINT ( 'NONE',  ( -25.98076211353310683, 55.53749999808803040, -3.000000000000132339 ) ) ;
#3422 = EDGE_CURVE ( 'NONE', #4007, #9236, #6751, .T. ) ;
#3423 = CARTESIAN_POINT ( 'NONE',  ( 15.87890888817147150, 17.65662501776163040, 12.17661548709639341 ) ) ;
#3424 = CARTESIAN_POINT ( 'NONE',  ( -25.17020516978313083, 54.03541666571061342, -6.403925809002825709 ) ) ;
#3425 = ADVANCED_FACE ( 'NONE', ( #9367 ), #1078, .T. ) ;
#3426 = CARTESIAN_POINT ( 'NONE',  ( 24.49999999999999289, -1.232050807568863426, -4.999999999999992006 ) ) ;
#3427 = CARTESIAN_POINT ( 'NONE',  ( 2.500000000000000000, 2.357898499370433054, -1.951563910473907981E-15 ) ) ;
#3428 = DIRECTION ( 'NONE',  ( -1.000000000000000000, -0.000000000000000000, -0.000000000000000000 ) ) ;
#3429 = VERTEX_POINT ( 'NONE', #7037 ) ;
#3430 = FACE_OUTER_BOUND ( 'NONE', #486, .T. ) ;
#3431 = DIRECTION ( 'NONE',  ( -0.000000000000000000, 0.000000000000000000, 1.000000000000000000 ) ) ;
#3432 =( BOUNDED_CURVE ( )  B_SPLINE_CURVE ( 2, ( #5491, #1938, #311, #3598, #2773, #7095, #4605, #7987, #2879 ),
 .UNSPECIFIED., .F., .F. ) 
 B_SPLINE_CURVE_WITH_KNOTS ( ( 3, 2, 2, 2, 3 ),
 ( 0.7500000000000000000, 0.7592592592592593004, 0.7777777777777777901, 0.7962962962962962798, 0.8055555555555555802 ),
 .UNSPECIFIED. ) 
 CURVE ( )  GEOMETRIC_REPRESENTATION_ITEM ( )  RATIONAL_B_SPLINE_CURVE ( ( 0.9330127018922194093, 0.9330127018922194093, 1.000000000000000000, 0.8660254037844387076, 1.000000000000000000, 0.8660254037844387076, 1.000000000000000000, 0.9330127018922189652, 0.9330127018922194093 ) ) 
 REPRESENTATION_ITEM ( '' )  );
#3433 = CARTESIAN_POINT ( 'NONE',  ( -25.17020516978313083, 52.57708333237728482, -3.596074190997380349 ) ) ;
#3434 = EDGE_CURVE ( 'NONE', #3095, #8941, #3542, .T. ) ;
#3435 = DIRECTION ( 'NONE',  ( 0.000000000000000000, 0.000000000000000000, 1.000000000000000000 ) ) ;
#3436 = EDGE_CURVE ( 'NONE', #10149, #4955, #6033, .T. ) ;
#3437 = LINE ( 'NONE', #7603, #5724 ) ;
#3438 = CARTESIAN_POINT ( 'NONE',  ( -27.98076211353308551, 51.30833333333320212, -3.845299461620869330 ) ) ;
#3439 = ORIENTED_EDGE ( 'NONE', *, *, #1240, .T. ) ;
#3440 = ORIENTED_EDGE ( 'NONE', *, *, #4707, .T. ) ;
#3441 = CARTESIAN_POINT ( 'NONE',  ( 15.87890888817147150, 17.65662501776163040, 12.17661548709639341 ) ) ;
#3442 = VERTEX_POINT ( 'NONE', #6084 ) ;
#3443 = CONICAL_SURFACE ( 'NONE', #5025, 3.499999999999999556, 1.047197551196603849 ) ;
#3444 = CARTESIAN_POINT ( 'NONE',  ( 3.199999999999999734, 0.000000000000000000, -3.499999999999999556 ) ) ;
#3445 = CARTESIAN_POINT ( 'NONE',  ( -38.99999999999986500, -3.999999999999940936, -5.000000000000027534 ) ) ;
#3446 = EDGE_LOOP ( 'NONE', ( #9862, #2058, #1946, #9965 ) ) ;
#3447 = CARTESIAN_POINT ( 'NONE',  ( 23.17052989764754756, 21.62756661655841839, 12.00579112326981246 ) ) ;
#3448 = DIRECTION ( 'NONE',  ( -0.000000000000000000, -0.000000000000000000, -1.000000000000000000 ) ) ;
#3449 = DIRECTION ( 'NONE',  ( -1.000000000000000000, -0.000000000000000000, -0.000000000000000000 ) ) ;
#3450 =( REPRESENTATION_RELATIONSHIP ('NONE','NONE', #7540, #10603 ) REPRESENTATION_RELATIONSHIP_WITH_TRANSFORMATION ( #9654 )SHAPE_REPRESENTATION_RELATIONSHIP( ) );
#3451 = CARTESIAN_POINT ( 'NONE',  ( -25.98076211353311393, 50.06874999904394485, -6.871901078670400231 ) ) ;
#3452 = CARTESIAN_POINT ( 'NONE',  ( 22.60611905166032898, 18.24656216730335601, 11.95042449705224819 ) ) ;
#3453 = VECTOR ( 'NONE', #7609, 1000.000000000000000 ) ;
#3454 = CARTESIAN_POINT ( 'NONE',  ( -1.449747468305836229, 33.50000000000000000, 16.23437500000000355 ) ) ;
#3455 = CARTESIAN_POINT ( 'NONE',  ( -26.79131905728310059, 50.12708333237728198, -6.403925809002825709 ) ) ;
#3456 = CARTESIAN_POINT ( 'NONE',  ( -25.98076211353324894, 14.99999999999984190, 2.500000000000000000 ) ) ;
#3457 = EDGE_LOOP ( 'NONE', ( #9378, #4513, #10645, #2408 ) ) ;
#3458 = CARTESIAN_POINT ( 'NONE',  ( -25.18320465585345502, 58.61672392917972729, -3.163343793118901903 ) ) ;
#3459 = VERTEX_POINT ( 'NONE', #3592 ) ;
#3460 = CARTESIAN_POINT ( 'NONE',  ( 2.474873734152918558, 32.47487373415292211, 16.00000000000000355 ) ) ;
#3461 = VECTOR ( 'NONE', #9188, 1000.000000000000000 ) ;
#3462 = ORIENTED_EDGE ( 'NONE', *, *, #8656, .T. ) ;
#3463 = CARTESIAN_POINT ( 'NONE',  ( 15.17335179141131185, 18.36218211452176519, 12.24278471274156388 ) ) ;
#3464 = AXIS2_PLACEMENT_3D ( 'NONE', #7721, #41, #8493 ) ;
#3465 = CARTESIAN_POINT ( 'NONE',  ( 16.72700999897183038, 16.80849948458634557, 12.09707671258119888 ) ) ;
#3466 = CARTESIAN_POINT ( 'NONE',  ( 17.86810043078960319, 17.16701444005803268, 12.06109941161078325 ) ) ;
#3467 = CARTESIAN_POINT ( 'NONE',  ( -27.60187600103308370, 50.76874999904395480, -5.000000000000103029 ) ) ;
#3468 = AXIS2_PLACEMENT_3D ( 'NONE', #6756, #5105, #10154 ) ;
#3469 = CARTESIAN_POINT ( 'NONE',  ( -2.385244779468109755E-15, 32.50000000000000711, 13.65625000000000355 ) ) ;
#3470 = CIRCLE ( 'NONE', #5420, 4.000000000000000000 ) ;
#3471 = DIRECTION ( 'NONE',  ( -1.000000000000000000, -0.000000000000000000, -0.000000000000000000 ) ) ;
#3472 = CARTESIAN_POINT ( 'NONE',  ( 29.50000000000000711, -9.999999999999998224, -10.50000000000001243 ) ) ;
#3473 = ORIENTED_EDGE ( 'NONE', *, *, #8406, .T. ) ;
#3474 = VERTEX_POINT ( 'NONE', #10424 ) ;
#3475 = CARTESIAN_POINT ( 'NONE',  ( -27.98076211353308551, 51.89166666666653782, -6.154700538379338504 ) ) ;
#3476 = VECTOR ( 'NONE', #3178, 1000.000000000000000 ) ;
#3477 = LINE ( 'NONE', #6797, #5625 ) ;
#3478 = CARTESIAN_POINT ( 'NONE',  ( 34.89259351528886555, 2.743407123163640104, -3.513512538347002057 ) ) ;
#3479 = CIRCLE ( 'NONE', #4369, 1.649999999999989919 ) ;
#3480 = CARTESIAN_POINT ( 'NONE',  ( 0.2500000000000002220, 4.898587196589412829E-16, -4.000000000000000000 ) ) ;
#3481 = DIRECTION ( 'NONE',  ( 0.000000000000000000, 1.000000000000000000, -1.471414886128461471E-15 ) ) ;
#3482 = CARTESIAN_POINT ( 'NONE',  ( -25.98076211353311393, 54.79374999904395338, -6.871901078670400231 ) ) ;
#3483 = DIRECTION ( 'NONE',  ( 0.000000000000000000, 0.000000000000000000, -1.000000000000000000 ) ) ;
#3484 = LINE ( 'NONE', #4317, #10204 ) ;
#3485 = CARTESIAN_POINT ( 'NONE',  ( 4.200000000000001954, 2.694222958124178486E-16, 2.200000000000001066 ) ) ;
#3486 = ORIENTED_EDGE ( 'NONE', *, *, #2003, .F. ) ;
#3487 = VECTOR ( 'NONE', #8740, 1000.000000000000114 ) ;
#3488 = LINE ( 'NONE', #6870, #151 ) ;
#3489 = CARTESIAN_POINT ( 'NONE',  ( -25.17020516978313083, 52.11041666571060915, -6.403925809002825709 ) ) ;
#3490 = CARTESIAN_POINT ( 'NONE',  ( -25.44486372867087809, 50.75626073911681857, -3.000000000000133671 ) ) ;
#3491 = AXIS2_PLACEMENT_3D ( 'NONE', #102, #5490, #1833 ) ;
#3492 = DIRECTION ( 'NONE',  ( 0.000000000000000000, 0.000000000000000000, 1.000000000000000000 ) ) ;
#3493 = CARTESIAN_POINT ( 'NONE',  ( -26.98076211353309972, 54.86666666666653214, -3.267949192431252037 ) ) ;
#3494 = VERTEX_POINT ( 'NONE', #81 ) ;
#3495 = EDGE_CURVE ( 'NONE', #9475, #5073, #3479, .T. ) ;
#3496 = ORIENTED_EDGE ( 'NONE', *, *, #7423, .T. ) ;
#3497 = DIRECTION ( 'NONE',  ( 1.000000000000000000, 0.000000000000000000, 0.000000000000000000 ) ) ;
#3498 = EDGE_CURVE ( 'NONE', #9249, #7102, #191, .T. ) ;
#3499 = CYLINDRICAL_SURFACE ( 'NONE', #8413, 7.500000000000000000 ) ;
#3500 = SHAPE_DEFINITION_REPRESENTATION ( #6780, #5283 ) ;
#3501 = ORIENTED_EDGE ( 'NONE', *, *, #5607, .T. ) ;
#3502 = CARTESIAN_POINT ( 'NONE',  ( 18.79784185921769790, 16.99560944861731215, 12.01584860934582366 ) ) ;
#3503 = CARTESIAN_POINT ( 'NONE',  ( 3.510273485745307731, 2.827716139362654424, -3.610536846335885564 ) ) ;
#3504 = LINE ( 'NONE', #5335, #7016 ) ;
#3505 =( GEOMETRIC_REPRESENTATION_CONTEXT ( 3 ) GLOBAL_UNCERTAINTY_ASSIGNED_CONTEXT ( ( #1562 ) ) GLOBAL_UNIT_ASSIGNED_CONTEXT ( ( #2671, #6885, #1950 ) ) REPRESENTATION_CONTEXT ( 'NONE', 'WORKASPACE' ) );
#3506 = LINE ( 'NONE', #4110, #834 ) ;
#3507 = CARTESIAN_POINT ( 'NONE',  ( 16.86040243112223180, 16.67515725582037689, 11.08237315523004973 ) ) ;
#3508 = CARTESIAN_POINT ( 'NONE',  ( -2.344047193898593395, -3.265465875126480455, -1.054683074273691752E-14 ) ) ;
#3509 = CARTESIAN_POINT ( 'NONE',  ( -27.98076211353308551, 54.66249999808803040, -5.000000000000103029 ) ) ;
#3510 = EDGE_CURVE ( 'NONE', #9249, #5721, #2761, .T. ) ;
#3511 = DIRECTION ( 'NONE',  ( -1.000000000000000000, 0.000000000000000000, 0.000000000000000000 ) ) ;
#3512 = ORIENTED_EDGE ( 'NONE', *, *, #4393, .T. ) ;
#3513 = LINE ( 'NONE', #3673, #1207 ) ;
#3514 = ORIENTED_EDGE ( 'NONE', *, *, #6957, .F. ) ;
#3515 = CONICAL_SURFACE ( 'NONE', #5800, 4.000000000000000000, 0.8911886515913786111 ) ;
#3516 = CARTESIAN_POINT ( 'NONE',  ( -1.449747468305836229, 33.50000000000000000, 16.23437500000000355 ) ) ;
#3517 = ORIENTED_EDGE ( 'NONE', *, *, #5228, .T. ) ;
#3518 = CARTESIAN_POINT ( 'NONE',  ( 17.78598590678423719, 16.10215687441832699, 12.01726674494117653 ) ) ;
#3519 = EDGE_CURVE ( 'NONE', #927, #1487, #10573, .T. ) ;
#3520 = CARTESIAN_POINT ( 'NONE',  ( 20.15426471261298147, 16.54100339847095213, 11.95042283504686154 ) ) ;
#3521 = VECTOR ( 'NONE', #5451, 1000.000000000000000 ) ;
#3522 = MECHANICAL_DESIGN_GEOMETRIC_PRESENTATION_REPRESENTATION (  '', ( #4233 ), #4041 ) ;
#3523 = CARTESIAN_POINT ( 'NONE',  ( 22.29575558078030895, 19.24694448270711788, 12.00579112326941988 ) ) ;
#3524 = CARTESIAN_POINT ( 'NONE',  ( -27.60187600103308014, 50.82708333237729192, -4.064049460664955760 ) ) ;
#3525 =( GEOMETRIC_REPRESENTATION_CONTEXT ( 3 ) GLOBAL_UNCERTAINTY_ASSIGNED_CONTEXT ( ( #2190 ) ) GLOBAL_UNIT_ASSIGNED_CONTEXT ( ( #401, #8748, #4594 ) ) REPRESENTATION_CONTEXT ( 'NONE', 'WORKASPACE' ) );
#3526 = CARTESIAN_POINT ( 'NONE',  ( -2.500000000000005773, 29.99999999999999645, 15.21875000000000355 ) ) ;
#3527 = LINE ( 'NONE', #7576, #7903 ) ;
#3528 = PLANE ( 'NONE',  #10429 ) ;
#3529 = VERTEX_POINT ( 'NONE', #1930 ) ;
#3530 = ORIENTED_EDGE ( 'NONE', *, *, #7024, .T. ) ;
#3531 = EDGE_CURVE ( 'NONE', #381, #9804, #6924, .T. ) ;
#3532 = VECTOR ( 'NONE', #1120, 1000.000000000000000 ) ;
#3533 = CARTESIAN_POINT ( 'NONE',  ( 17.65010306112908722, 17.31038946799904465, 12.07741653513508417 ) ) ;
#3534 = DIRECTION ( 'NONE',  ( 1.000000000000000000, 0.000000000000000000, 0.000000000000000000 ) ) ;
#3535 = VECTOR ( 'NONE', #9334, 1000.000000000000000 ) ;
#3536 = CARTESIAN_POINT ( 'NONE',  ( 22.82387490247590733, 19.65457484615246386, 12.00579112326941988 ) ) ;
#3537 = CARTESIAN_POINT ( 'NONE',  ( -26.51666049839534978, 52.79373926088290148, -3.000000000000133227 ) ) ;
#3538 = DIRECTION ( 'NONE',  ( 0.000000000000000000, -1.000000000000000000, -0.000000000000000000 ) ) ;
#3539 = CARTESIAN_POINT ( 'NONE',  ( -25.98076211353311393, 53.74374999904394912, -3.128098921329806714 ) ) ;
#3540 = DIRECTION ( 'NONE',  ( -1.000000000000000000, -0.000000000000000000, -0.000000000000000000 ) ) ;
#3541 = DIRECTION ( 'NONE',  ( 0.000000000000000000, 0.000000000000000000, -1.000000000000000000 ) ) ;
#3542 = LINE ( 'NONE', #9530, #1158 ) ;
#3543 = ORIENTED_EDGE ( 'NONE', *, *, #4402, .F. ) ;
#3544 = LINE ( 'NONE', #3645, #6703 ) ;
#3545 = CARTESIAN_POINT ( 'NONE',  ( 0.06616922564517249694, 32.50000000000000711, 17.15405841526694175 ) ) ;
#3546 = CARTESIAN_POINT ( 'NONE',  ( 0.000000000000000000, -2.357898499370432610, 3.252606517456513302E-15 ) ) ;
#3547 = CARTESIAN_POINT ( 'NONE',  ( -24.35964822603314772, 55.55208333237727913, -5.935950539335252074 ) ) ;
#3548 = DIRECTION ( 'NONE',  ( 0.000000000000000000, 1.000000000000000000, 0.000000000000000000 ) ) ;
#3549 = CARTESIAN_POINT ( 'NONE',  ( -25.98076211353311393, 49.49999999999986500, -3.000000000000131894 ) ) ;
#3550 = CARTESIAN_POINT ( 'NONE',  ( -27.98076211353308551, 55.39166666666653072, -6.154700538379338504 ) ) ;
#3551 = EDGE_LOOP ( 'NONE', ( #6107, #6565, #9396 ) ) ;
#3552 = EDGE_CURVE ( 'NONE', #4884, #7995, #1348, .T. ) ;
#3553 = ORIENTED_EDGE ( 'NONE', *, *, #9790, .T. ) ;
#3554 = CARTESIAN_POINT ( 'NONE',  ( 5.200000000000002842, 0.000000000000000000, 0.000000000000000000 ) ) ;
#3555 = LINE ( 'NONE', #2495, #5411 ) ;
#3556 = DIRECTION ( 'NONE',  ( 0.000000000000000000, 0.000000000000000000, 1.000000000000000000 ) ) ;
#3557 = ORIENTED_EDGE ( 'NONE', *, *, #10421, .F. ) ;
#3558 = CARTESIAN_POINT ( 'NONE',  ( 2.887392608830349428, 4.041451884327400101, -2.289061810243902218E-14 ) ) ;
#3559 = CARTESIAN_POINT ( 'NONE',  ( -23.98076211353314235, 54.39999999999986358, -5.000000000000103029 ) ) ;
#3560 = EDGE_CURVE ( 'NONE', #381, #7106, #6138, .T. ) ;
#3561 = CARTESIAN_POINT ( 'NONE',  ( 16.67998965505631404, 16.85551971246726310, 11.09929001438087148 ) ) ;
#3562 = CARTESIAN_POINT ( 'NONE',  ( -4.000000000000000000, -2.309401076758512694, -3.433295621305382461 ) ) ;
#3563 = EDGE_CURVE ( 'NONE', #8370, #3879, #8587, .T. ) ;
#3564 = CARTESIAN_POINT ( 'NONE',  ( -24.35964822603314772, 52.75208333237727487, -5.935950539335252074 ) ) ;
#3565 = DIRECTION ( 'NONE',  ( 0.000000000000000000, 0.000000000000000000, -1.000000000000000000 ) ) ;
#3566 = ORIENTED_EDGE ( 'NONE', *, *, #10229, .T. ) ;
#3567 = CARTESIAN_POINT ( 'NONE',  ( -2.499999999999999556, 3.061616997868382648E-16, 3.469446951953614189E-15 ) ) ;
#3568 = ORIENTED_EDGE ( 'NONE', *, *, #4103, .F. ) ;
#3569 = CARTESIAN_POINT ( 'NONE',  ( -1.515916693951010252, 33.47259180932604750, 15.23656658473306535 ) ) ;
#3570 = ORIENTED_EDGE ( 'NONE', *, *, #10590, .T. ) ;
#3571 = CARTESIAN_POINT ( 'NONE',  ( 22.47621881040483771, 18.15620256126511478, 11.95042449705224819 ) ) ;
#3572 = EDGE_CURVE ( 'NONE', #8904, #7419, #10754, .T. ) ;
#3573 = CARTESIAN_POINT ( 'NONE',  ( 24.32342464814431438, 20.41340561598360992, 11.95042449705224996 ) ) ;
#3574 = CARTESIAN_POINT ( 'NONE',  ( 23.04535143233503192, 19.92821688535955360, 12.00579112326941988 ) ) ;
#3575 = CARTESIAN_POINT ( 'NONE',  ( -25.98076211353311393, 50.59374999904395054, -6.871901078670400231 ) ) ;
#3576 = VECTOR ( 'NONE', #2358, 1000.000000000000000 ) ;
#3577 = CARTESIAN_POINT ( 'NONE',  ( 2.500000000000000000, 2.357898499370433054, -1.951563910473907981E-15 ) ) ;
#3578 = DIRECTION ( 'NONE',  ( 0.000000000000000000, 1.000000000000000000, 0.000000000000000000 ) ) ;
#3579 = CARTESIAN_POINT ( 'NONE',  ( -26.98076211353408382, 57.99999999999985789, -6.732050807568389139 ) ) ;
#3580 = EDGE_CURVE ( 'NONE', #1107, #3494, #1815, .T. ) ;
#3581 = ORIENTED_EDGE ( 'NONE', *, *, #749, .T. ) ;
#3582 = EDGE_CURVE ( 'NONE', #433, #6171, #914, .T. ) ;
#3583 = ORIENTED_EDGE ( 'NONE', *, *, #7475, .T. ) ;
#3584 = PLANE ( 'NONE',  #8096 ) ;
#3585 = CIRCLE ( 'NONE', #6947, 1.649999999999998579 ) ;
#3586 = DIRECTION ( 'NONE',  ( 0.000000000000000000, 0.000000000000000000, -1.000000000000000000 ) ) ;
#3587 = DIRECTION ( 'NONE',  ( 0.000000000000000000, -1.000000000000000000, 0.000000000000000000 ) ) ;
#3588 = LINE ( 'NONE', #8025, #6306 ) ;
#3589 = DIRECTION ( 'NONE',  ( -0.9009800080279036782, 0.000000000000000000, 0.4338606056489096585 ) ) ;
#3590 = CARTESIAN_POINT ( 'NONE',  ( -26.79131905728310059, 55.55208333237728624, -6.403925809002825709 ) ) ;
#3591 = DIRECTION ( 'NONE',  ( 0.000000000000000000, 0.000000000000000000, 1.000000000000000000 ) ) ;
#3592 = CARTESIAN_POINT ( 'NONE',  ( -2.500000000000000888, 0.000000000000000000, -4.974599999999998801 ) ) ;
#3593 = ORIENTED_EDGE ( 'NONE', *, *, #635, .T. ) ;
#3594 = CARTESIAN_POINT ( 'NONE',  ( -1.035533905932742638, 32.50000000000000000, 14.98437500000000711 ) ) ;
#3595 = CARTESIAN_POINT ( 'NONE',  ( -2.385244779468109755E-15, 32.50000000000000711, 14.90625000000000355 ) ) ;
#3596 = CIRCLE ( 'NONE', #558, 2.149999999999995470 ) ;
#3597 = EDGE_CURVE ( 'NONE', #38, #8106, #7449, .T. ) ;
#3598 = CARTESIAN_POINT ( 'NONE',  ( -23.98076211353314235, 54.95416666475470180, -3.845299461620867554 ) ) ;
#3599 = EDGE_CURVE ( 'NONE', #9170, #8106, #985, .T. ) ;
#3600 = DIRECTION ( 'NONE',  ( 0.000000000000000000, 0.000000000000000000, 1.000000000000000000 ) ) ;
#3601 = CARTESIAN_POINT ( 'NONE',  ( -30.75045812061784289, 16.50000000000026290, -5.000000000000000000 ) ) ;
#3602 = CARTESIAN_POINT ( 'NONE',  ( 0.02539999999999975264, 2.449293598294706414E-16, 2.000000000000000000 ) ) ;
#3603 = CIRCLE ( 'NONE', #4498, 4.500000000000000000 ) ;
#3604 = ORIENTED_EDGE ( 'NONE', *, *, #1272, .T. ) ;
#3605 = ORIENTED_EDGE ( 'NONE', *, *, #8138, .T. ) ;
#3606 = CARTESIAN_POINT ( 'NONE',  ( -25.98076211353311393, 54.57499999999986073, -7.000000000000072831 ) ) ;
#3607 = DIRECTION ( 'NONE',  ( -1.000000000000000000, -0.000000000000000000, -0.000000000000000000 ) ) ;
#3608 = VERTEX_POINT ( 'NONE', #9696 ) ;
#3609 = DIRECTION ( 'NONE',  ( 0.000000000000000000, 0.000000000000000000, 1.000000000000000000 ) ) ;
#3610 = LINE ( 'NONE', #936, #3993 ) ;
#3611 = CARTESIAN_POINT ( 'NONE',  ( 16.45601903647678910, 17.07951486945825792, 11.12029599681952519 ) ) ;
#3612 = CARTESIAN_POINT ( 'NONE',  ( -3.500000000000003109, 29.99999999999999645, 16.46875000000000355 ) ) ;
#3613 = CARTESIAN_POINT ( 'NONE',  ( -27.60187600103308014, 52.98541666571061626, -5.935950539335252074 ) ) ;
#3614 = DIRECTION ( 'NONE',  ( 0.000000000000000000, 1.000000000000000000, 0.000000000000000000 ) ) ;
#3615 = ORIENTED_EDGE ( 'NONE', *, *, #3083, .F. ) ;
#3616 = DIRECTION ( 'NONE',  ( -0.7055570967602537991, 0.7055570967602550203, 0.06616922564517474514 ) ) ;
#3617 = VERTEX_POINT ( 'NONE', #10687 ) ;
#3618 = CARTESIAN_POINT ( 'NONE',  ( 1.101703131577918438, 27.52740819067395606, 14.61156658473306713 ) ) ;
#3619 = EDGE_LOOP ( 'NONE', ( #7612, #5782, #4671, #8662, #1868 ) ) ;
#3620 = CARTESIAN_POINT ( 'NONE',  ( 23.64018263364375017, 19.06693133664117212, 11.95042449705224819 ) ) ;
#3621 = SURFACE_STYLE_FILL_AREA ( #1909 ) ;
#3622 = VECTOR ( 'NONE', #7720, 1000.000000000000000 ) ;
#3623 = CARTESIAN_POINT ( 'NONE',  ( 0.000000000000000000, 0.000000000000000000, -5.000000000000000000 ) ) ;
#3624 = CARTESIAN_POINT ( 'NONE',  ( 19.85760542366876535, 20.31250532737884384, 12.00579112326941988 ) ) ;
#3625 = CARTESIAN_POINT ( 'NONE',  ( -24.35964822603314772, 50.36041666571061626, -4.064049460664953983 ) ) ;
#3626 = CARTESIAN_POINT ( 'NONE',  ( -4.000000000000004441, 2.309401076758496263, -3.504269196027523847 ) ) ;
#3627 = LINE ( 'NONE', #10350, #6473 ) ;
#3628 = CYLINDRICAL_SURFACE ( 'NONE', #9173, 1.999999999999971356 ) ;
#3629 = ORIENTED_EDGE ( 'NONE', *, *, #1622, .F. ) ;
#3630 = EDGE_CURVE ( 'NONE', #3617, #1228, #10736, .T. ) ;
#3631 = ORIENTED_EDGE ( 'NONE', *, *, #9460, .T. ) ;
#3632 = CIRCLE ( 'NONE', #426, 1.535500000000000087 ) ;
#3633 = EDGE_CURVE ( 'NONE', #8370, #4598, #10732, .T. ) ;
#3634 = DIRECTION ( 'NONE',  ( -0.000000000000000000, -1.000000000000000000, -0.000000000000000000 ) ) ;
#3635 = CARTESIAN_POINT ( 'NONE',  ( 2.500000000000000444, 0.000000000000000000, -25.03750572909317285 ) ) ;
#3636 = DIRECTION ( 'NONE',  ( 0.000000000000000000, 0.000000000000000000, -1.000000000000000000 ) ) ;
#3637 = AXIS2_PLACEMENT_3D ( 'NONE', #10539, #2934, #10433 ) ;
#3638 = CARTESIAN_POINT ( 'NONE',  ( -27.78269984933782411, 56.11211482050297406, -4.132232521764788835 ) ) ;
#3639 = AXIS2_PLACEMENT_3D ( 'NONE', #9070, #5792, #8347 ) ;
#3640 = DIRECTION ( 'NONE',  ( 1.000000000000000000, 0.000000000000000000, 0.000000000000000000 ) ) ;
#3641 = DIRECTION ( 'NONE',  ( 1.000000000000000000, -0.000000000000000000, -0.000000000000000000 ) ) ;
#3642 = CARTESIAN_POINT ( 'NONE',  ( -3.500000000000003109, 29.99999999999999645, 16.46875000000000355 ) ) ;
#3643 = CARTESIAN_POINT ( 'NONE',  ( 5.076455387921338769, 24.47916666666667140, 0.000000000000000000 ) ) ;
#3644 = EDGE_LOOP ( 'NONE', ( #8151, #3583, #2182, #10689 ) ) ;
#3645 = CARTESIAN_POINT ( 'NONE',  ( -30.75045812061784289, 16.50000000000026290, -9.500000000000000000 ) ) ;
#3646 = AXIS2_PLACEMENT_3D ( 'NONE', #6324, #5386, #8771 ) ;
#3647 = CARTESIAN_POINT ( 'NONE',  ( -2.527408190673963162, 29.03063531971243094, 15.04468341526694175 ) ) ;
#3648 = FACE_OUTER_BOUND ( 'NONE', #3929, .T. ) ;
#3649 = UNCERTAINTY_MEASURE_WITH_UNIT (LENGTH_MEASURE( 1.000000000000000082E-05 ), #3017, 'distance_accuracy_value', 'NONE');
#3650 = VECTOR ( 'NONE', #8862, 1000.000000000000000 ) ;
#3651 = CIRCLE ( 'NONE', #2229, 0.4999999999999981681 ) ;
#3652 = DIRECTION ( 'NONE',  ( 0.000000000000000000, 0.000000000000000000, -1.000000000000000000 ) ) ;
#3653 = CARTESIAN_POINT ( 'NONE',  ( -23.98076211353314235, 52.94166666666653498, -3.845299461620867554 ) ) ;
#3654 = AXIS2_PLACEMENT_3D ( 'NONE', #7924, #2979, #6354 ) ;
#3655 = CARTESIAN_POINT ( 'NONE',  ( 3.078243469714894598, 2.351289329882122914, -2.927447417349547720 ) ) ;
#3656 = CARTESIAN_POINT ( 'NONE',  ( 34.99999999999999289, -3.999999999999993339, -4.999999999999995559 ) ) ;
#3657 = AXIS2_PLACEMENT_3D ( 'NONE', #1305, #2189, #10644 ) ;
#3658 = ORIENTED_EDGE ( 'NONE', *, *, #9220, .T. ) ;
#3659 = ORIENTED_EDGE ( 'NONE', *, *, #7703, .F. ) ;
#3660 = CARTESIAN_POINT ( 'NONE',  ( 0.000000000000000000, 5.051668046482832750E-16, -4.000000000000000000 ) ) ;
#3661 = PLANE ( 'NONE',  #5585 ) ;
#3662 = APPLICATION_PROTOCOL_DEFINITION ( 'draft international standard', 'automotive_design', 1998, #530 ) ;
#3663 = ORIENTED_EDGE ( 'NONE', *, *, #8236, .T. ) ;
#3664 = ADVANCED_FACE ( 'NONE', ( #8082 ), #10533, .T. ) ;
#3665 = DIRECTION ( 'NONE',  ( -1.000000000000000000, -0.000000000000000000, -0.000000000000000000 ) ) ;
#3666 = AXIS2_PLACEMENT_3D ( 'NONE', #7990, #4768, #1203 ) ;
#3667 = CARTESIAN_POINT ( 'NONE',  ( 0.2174200650117590894, -3.876582599186223721, -0.2855619784720447862 ) ) ;
#3668 = CARTESIAN_POINT ( 'NONE',  ( 16.30404126228686579, 18.64570620602049189, 11.20086348037537327 ) ) ;
#3669 = DIRECTION ( 'NONE',  ( -4.312387734421975126E-17, 0.7071067811865451302, -0.7071067811865500152 ) ) ;
#3670 = CARTESIAN_POINT ( 'NONE',  ( -27.60187600103308014, 54.50208333237726777, -4.064049460664955760 ) ) ;
#3671 = DIRECTION ( 'NONE',  ( -1.000000000000000000, -0.000000000000000000, -0.000000000000000000 ) ) ;
#3672 = EDGE_LOOP ( 'NONE', ( #5769, #130 ) ) ;
#3673 = CARTESIAN_POINT ( 'NONE',  ( 34.99999999999987210, -3.999999999999989786, 7.850000000000005862 ) ) ;
#3674 = ORIENTED_EDGE ( 'NONE', *, *, #4582, .F. ) ;
#3675 = CARTESIAN_POINT ( 'NONE',  ( 2.500000000000006661, 30.06616922564517580, 13.59594158473306358 ) ) ;
#3676 = EDGE_LOOP ( 'NONE', ( #10863, #2565, #9321, #10103 ) ) ;
#3677 = CARTESIAN_POINT ( 'NONE',  ( 24.09141472773967507, 22.06251279622207306, 11.95042449705264076 ) ) ;
#3678 = CARTESIAN_POINT ( 'NONE',  ( -27.60187600103308370, 50.94374999904394485, -5.000000000000103029 ) ) ;
#3679 =( NAMED_UNIT ( * ) SI_UNIT ( $, .STERADIAN. ) SOLID_ANGLE_UNIT ( ) );
#3680 = CARTESIAN_POINT ( 'NONE',  ( 29.49999999999999645, -8.499999999999985789, -4.999999999999991118 ) ) ;
#3681 = CARTESIAN_POINT ( 'NONE',  ( 15.22014049957087956, 18.31539340636219393, 13.24059312800850030 ) ) ;
#3682 = CARTESIAN_POINT ( 'NONE',  ( -25.17020516978313083, 54.73541666571062336, -6.403925809002825709 ) ) ;
#3683 = AXIS2_PLACEMENT_3D ( 'NONE', #708, #10942, #5943 ) ;
#3684 = CARTESIAN_POINT ( 'NONE',  ( 29.50000000000000711, 2.000000000000001776, -12.50000000000000000 ) ) ;
#3685 = CARTESIAN_POINT ( 'NONE',  ( 4.000000000000000000, 2.309401076758497151, -5.000000000000000000 ) ) ;
#3686 = EDGE_CURVE ( 'NONE', #5523, #4738, #8186, .T. ) ;
#3687 = ORIENTED_EDGE ( 'NONE', *, *, #3883, .T. ) ;
#3688 = CYLINDRICAL_SURFACE ( 'NONE', #5620, 5.000000000000000888 ) ;
#3689 = LINE ( 'NONE', #1974, #3650 ) ;
#3690 = AXIS2_PLACEMENT_3D ( 'NONE', #10631, #7858, #3022 ) ;
#3691 = STYLED_ITEM ( 'NONE', ( #1340 ), #3752 ) ;
#3692 = CARTESIAN_POINT ( 'NONE',  ( 0.1217565302850657921, -2.351289329882329859, -2.927447417349280823 ) ) ;
#3693 = CARTESIAN_POINT ( 'NONE',  ( -26.85339429124058697, 58.50531623421669281, -3.199529906863744166 ) ) ;
#3694 = CARTESIAN_POINT ( 'NONE',  ( -27.98076211353308551, 52.62083333142137320, -3.845299461620869330 ) ) ;
#3695 = DIRECTION ( 'NONE',  ( -1.000000000000000000, -0.000000000000000000, -0.000000000000000000 ) ) ;
#3696 = ADVANCED_FACE ( 'NONE', ( #7980, #6244 ), #7245, .F. ) ;
#3697 = CARTESIAN_POINT ( 'NONE',  ( -3.500000000000002220, 28.55025253169416288, 15.29687500000000178 ) ) ;
#3698 = DIRECTION ( 'NONE',  ( 1.000000000000000000, -0.000000000000000000, -0.000000000000000000 ) ) ;
#3699 = ORIENTED_EDGE ( 'NONE', *, *, #3371, .F. ) ;
#3700 = CARTESIAN_POINT ( 'NONE',  ( 34.99999999999999289, 2.000000000000002220, -12.49999999999999822 ) ) ;
#3701 = EDGE_CURVE ( 'NONE', #6726, #2280, #459, .T. ) ;
#3702 = CARTESIAN_POINT ( 'NONE',  ( -1.814555661125937247, 28.27902175519318817, 15.12280841526694353 ) ) ;
#3703 = AXIS2_PLACEMENT_3D ( 'NONE', #9870, #1476, #9035 ) ;
#3704 = CARTESIAN_POINT ( 'NONE',  ( -1.035533905932742638, 32.50000000000000000, 13.73437500000000533 ) ) ;
#3705 = CARTESIAN_POINT ( 'NONE',  ( 22.98009469009668138, 21.94211999725310491, 12.00579112326941988 ) ) ;
#3706 = CARTESIAN_POINT ( 'NONE',  ( -26.95340920277349284, 57.73396742993422492, -6.748466501715046029 ) ) ;
#3707 = CARTESIAN_POINT ( 'NONE',  ( -25.44486372867087809, 52.85626073911682710, -3.000000000000132339 ) ) ;
#3708 = ADVANCED_FACE ( 'NONE', ( #1191 ), #3032, .T. ) ;
#3709 = CARTESIAN_POINT ( 'NONE',  ( -25.17020516978313083, 52.81041666571061199, -6.403925809002825709 ) ) ;
#3710 = CARTESIAN_POINT ( 'NONE',  ( 6.015568632492056977, 34.47916666666665009, 2.500000000000000000 ) ) ;
#3711 = CARTESIAN_POINT ( 'NONE',  ( -23.98076211353314235, 54.45833333333320070, -6.154700538379337615 ) ) ;
#3712 = ORIENTED_EDGE ( 'NONE', *, *, #703, .T. ) ;
#3713 = EDGE_LOOP ( 'NONE', ( #9917, #6712 ) ) ;
#3714 = DIRECTION ( 'NONE',  ( -1.000000000000000000, -0.000000000000000000, -0.000000000000000000 ) ) ;
#3715 = EDGE_CURVE ( 'NONE', #6302, #12, #2555, .T. ) ;
#3716 = ADVANCED_FACE ( 'NONE', ( #4645 ), #617, .T. ) ;
#3717 = PLANE ( 'NONE',  #1864 ) ;
#3718 = PRODUCT_CONTEXT ( 'NONE', #530, 'mechanical' ) ;
#3719 = EDGE_LOOP ( 'NONE', ( #10446, #5642, #7450, #6398, #1407 ) ) ;
#3720 = CARTESIAN_POINT ( 'NONE',  ( -27.78269984933782411, 56.11211482050296695, -4.132232521764788835 ) ) ;
#3721 = CARTESIAN_POINT ( 'NONE',  ( -25.17020516978313083, 50.30208333237728624, -3.596074190997380349 ) ) ;
#3722 = CARTESIAN_POINT ( 'NONE',  ( 23.31046218964701211, 18.81639786330068276, 10.95195840513859231 ) ) ;
#3723 = VERTEX_POINT ( 'NONE', #1361 ) ;
#3724 = CARTESIAN_POINT ( 'NONE',  ( -27.60187600103308370, 53.74374999904394201, -5.000000000000103029 ) ) ;
#3725 = VERTEX_POINT ( 'NONE', #352 ) ;
#3726 = DIRECTION ( 'NONE',  ( -1.000000000000000000, 0.000000000000000000, 0.000000000000000000 ) ) ;
#3727 = VERTEX_POINT ( 'NONE', #403 ) ;
#3728 = CARTESIAN_POINT ( 'NONE',  ( -1.767766952966370209, 28.23223304703362402, 14.12500000000000355 ) ) ;
#3729 = VERTEX_POINT ( 'NONE', #3958 ) ;
#3730 = CARTESIAN_POINT ( 'NONE',  ( 18.92159813099251053, 21.64660971755233732, 10.95195840513820151 ) ) ;
#3731 =( NAMED_UNIT ( * ) PLANE_ANGLE_UNIT ( ) SI_UNIT ( $, .RADIAN. ) );
#3732 = EDGE_CURVE ( 'NONE', #1959, #10050, #2927, .T. ) ;
#3733 = DIRECTION ( 'NONE',  ( 0.000000000000000000, 0.000000000000000000, 1.000000000000000000 ) ) ;
#3734 = CARTESIAN_POINT ( 'NONE',  ( 17.07425424873056130, 16.47910233548095604, 13.06769463237219320 ) ) ;
#3735 = CARTESIAN_POINT ( 'NONE',  ( -27.60187600103308014, 55.61041666571061626, -5.935950539335252074 ) ) ;
#3736 = LINE ( 'NONE', #2912, #4232 ) ;
#3737 = CARTESIAN_POINT ( 'NONE',  ( -1.219727444046192735E-16, 2.000000000000000000, -10.50000000000000355 ) ) ;
#3738 = DIRECTION ( 'NONE',  ( -1.000000000000000000, -6.098637220230963674E-17, -1.156482317317871725E-16 ) ) ;
#3739 = EDGE_LOOP ( 'NONE', ( #474, #3123, #10175, #6714 ) ) ;
#3740 = ORIENTED_EDGE ( 'NONE', *, *, #8808, .F. ) ;
#3741 = CARTESIAN_POINT ( 'NONE',  ( 0.000000000000000000, 0.000000000000000000, 14.50000000000000000 ) ) ;
#3742 = FACE_BOUND ( 'NONE', #10708, .T. ) ;
#3743 = DIRECTION ( 'NONE',  ( 0.000000000000000000, 0.000000000000000000, -1.000000000000000000 ) ) ;
#3744 = ADVANCED_FACE ( 'NONE', ( #6300 ), #8137, .T. ) ;
#3745 = FACE_OUTER_BOUND ( 'NONE', #10501, .T. ) ;
#3746 = CARTESIAN_POINT ( 'NONE',  ( 25.49999999999999645, -3.999999999999986233, -3.349999999999993427 ) ) ;
#3747 = CARTESIAN_POINT ( 'NONE',  ( -25.98076211353311393, 52.73749999808803324, -3.000000000000132339 ) ) ;
#3748 = CARTESIAN_POINT ( 'NONE',  ( 34.99999999999999289, -9.999999999999998224, -10.50000000000000355 ) ) ;
#3749 = CARTESIAN_POINT ( 'NONE',  ( -23.98076211353314235, 49.49999999999986500, -5.000000000000103029 ) ) ;
#3750 = CARTESIAN_POINT ( 'NONE',  ( -0.06616922564517661864, 33.50000000000000000, 12.65844158473306535 ) ) ;
#3751 = CARTESIAN_POINT ( 'NONE',  ( -1.393927851585477606, 4.043713361053528743, -3.526374918436835149 ) ) ;
#3752 = ADVANCED_BREP_SHAPE_REPRESENTATION ( '', ( #1846, #308 ), #6179 ) ;
#3753 = ORIENTED_EDGE ( 'NONE', *, *, #1380, .T. ) ;
#3754 =( NAMED_UNIT ( * ) PLANE_ANGLE_UNIT ( ) SI_UNIT ( $, .RADIAN. ) );
#3755 = CARTESIAN_POINT ( 'NONE',  ( -0.9693646802875689472, 32.52740819067395961, 15.98218341526694175 ) ) ;
#3756 = CIRCLE ( 'NONE', #6617, 2.149999999999987921 ) ;
#3757 = CARTESIAN_POINT ( 'NONE',  ( 1.035533905932743970, 27.49999999999999289, 15.60937500000000711 ) ) ;
#3758 = DIRECTION ( 'NONE',  ( -0.4999999999999978906, -0.8660254037844399289, 1.424844972990615018E-16 ) ) ;
#3759 = ADVANCED_FACE ( 'NONE', ( #8030, #3913 ), #10589, .F. ) ;
#3760 = LINE ( 'NONE', #10487, #1327 ) ;
#3761 = CARTESIAN_POINT ( 'NONE',  ( 25.98076211353311749, 56.49999999999984368, 10.00000000000000178 ) ) ;
#3762 = EDGE_CURVE ( 'NONE', #7127, #3326, #4904, .T. ) ;
#3763 = EDGE_CURVE ( 'NONE', #7320, #6485, #5533, .T. ) ;
#3764 = CARTESIAN_POINT ( 'NONE',  ( -27.98076211353308551, 51.24999999999986500, -5.000000000000103029 ) ) ;
#3765 = CARTESIAN_POINT ( 'NONE',  ( -27.60187600103308014, 52.98541666571061626, -5.935950539335252074 ) ) ;
#3766 = LINE ( 'NONE', #4659, #1288 ) ;
#3767 = DIRECTION ( 'NONE',  ( 0.000000000000000000, 0.000000000000000000, 1.000000000000000000 ) ) ;
#3768 = ORIENTED_EDGE ( 'NONE', *, *, #9586, .F. ) ;
#3769 = EDGE_LOOP ( 'NONE', ( #4217, #4922, #2338, #587, #8729, #6322, #7664, #8390, #6381, #7736, #7365, #5368, #8945, #9292, #7163, #739, #6491, #4952, #7406, #10035, #4100 ) ) ;
#3770 = FACE_OUTER_BOUND ( 'NONE', #2019, .T. ) ;
#3771 = EDGE_CURVE ( 'NONE', #10326, #8941, #1173, .T. ) ;
#3772 = DIRECTION ( 'NONE',  ( 0.000000000000000000, -0.4999999999999922839, 0.8660254037844430375 ) ) ;
#3773 = ORIENTED_EDGE ( 'NONE', *, *, #2201, .F. ) ;
#3774 = EDGE_CURVE ( 'NONE', #170, #6485, #9690, .T. ) ;
#3775 = CARTESIAN_POINT ( 'NONE',  ( -4.000000000000000000, -2.309401076758512694, -3.433295621305382461 ) ) ;
#3776 = CARTESIAN_POINT ( 'NONE',  ( -24.35964822603314772, 49.77708333237728766, -5.935950539335252074 ) ) ;
#3777 = AXIS2_PLACEMENT_3D ( 'NONE', #6165, #6218, #2678 ) ;
#3778 = CARTESIAN_POINT ( 'NONE',  ( 18.81733698050991777, 21.09051435711097966, 10.95195840513859231 ) ) ;
#3779 = VERTEX_POINT ( 'NONE', #8400 ) ;
#3780 = CARTESIAN_POINT ( 'NONE',  ( -26.79131905728310059, 53.62708333237727487, -6.403925809002825709 ) ) ;
#3781 = EDGE_LOOP ( 'NONE', ( #1827, #1886, #3399 ) ) ;
#3782 = CARTESIAN_POINT ( 'NONE',  ( 5.621179405865841083, 34.96511249490581719, -2.499999999999999112 ) ) ;
#3783 = PRODUCT_DEFINITION_SHAPE ( 'NONE', 'NONE',  #11007 ) ;
#3784 = EDGE_LOOP ( 'NONE', ( #4150, #5129, #489, #832 ) ) ;
#3785 = CARTESIAN_POINT ( 'NONE',  ( -2.527408190673963162, 30.96936468028755840, 14.14281658473306713 ) ) ;
#3786 = ORIENTED_EDGE ( 'NONE', *, *, #1898, .F. ) ;
#3787 = CARTESIAN_POINT ( 'NONE',  ( 21.27550008773165047, 17.38841780631423362, 10.95195840513859231 ) ) ;
#3788 =( BOUNDED_CURVE ( )  B_SPLINE_CURVE ( 2, ( #8174, #4964, #9902, #6443, #3901, #2291, #1504, #10838, #8220 ),
 .UNSPECIFIED., .F., .F. ) 
 B_SPLINE_CURVE_WITH_KNOTS ( ( 3, 2, 2, 2, 3 ),
 ( 0.1388888888888888951, 0.1481481481481481399, 0.1666666666666666574, 0.1851851851851851749, 0.1944444444444444198 ),
 .UNSPECIFIED. ) 
 CURVE ( )  GEOMETRIC_REPRESENTATION_ITEM ( )  RATIONAL_B_SPLINE_CURVE ( ( 0.9330127018922192983, 0.9330127018922194093, 1.000000000000000000, 0.8660254037844387076, 1.000000000000000000, 0.8660254037844387076, 1.000000000000000000, 0.9330127018922194093, 0.9330127018922192983 ) ) 
 REPRESENTATION_ITEM ( '' )  );
#3789 = CYLINDRICAL_SURFACE ( 'NONE', #8123, 2.100000000000000089 ) ;
#3790 = CARTESIAN_POINT ( 'NONE',  ( 16.94475380574361623, 18.00499366256143219, 13.14516836485838169 ) ) ;
#3791 = CARTESIAN_POINT ( 'NONE',  ( -27.98076211353308551, 49.90833333333318933, -3.845299461620869330 ) ) ;
#3792 = PRESENTATION_STYLE_ASSIGNMENT (( #4577 ) ) ;
#3793 = CARTESIAN_POINT ( 'NONE',  ( 34.99999999999987210, -3.999999999999989786, -7.149999999999994138 ) ) ;
#3794 = ORIENTED_EDGE ( 'NONE', *, *, #5136, .T. ) ;
#3795 = EDGE_LOOP ( 'NONE', ( #10714, #4454, #10763, #2391 ) ) ;
#3796 = CARTESIAN_POINT ( 'NONE',  ( 20.17304365239387565, 21.99495017005343200, 12.00579112326981068 ) ) ;
#3797 = LINE ( 'NONE', #2136, #8992 ) ;
#3798 = CARTESIAN_POINT ( 'NONE',  ( -24.35964822603314417, 49.71874999904395054, -5.000000000000103029 ) ) ;
#3799 = CARTESIAN_POINT ( 'NONE',  ( -27.98076211353308551, 56.00416666475469896, -6.154700538379338504 ) ) ;
#3800 = CARTESIAN_POINT ( 'NONE',  ( 0.000000000000000000, 0.000000000000000000, 0.000000000000000000 ) ) ;
#3801 = LINE ( 'NONE', #299, #7775 ) ;
#3802 = CARTESIAN_POINT ( 'NONE',  ( 3.472591809326051937, 28.48408330604899419, 16.76343341526694175 ) ) ;
#3803 = DIRECTION ( 'NONE',  ( 0.000000000000000000, 0.8660254037844380415, -0.5000000000000011102 ) ) ;
#3804 = AXIS2_PLACEMENT_3D ( 'NONE', #6259, #4557, #2048 ) ;
#3805 = ORIENTED_EDGE ( 'NONE', *, *, #1740, .T. ) ;
#3806 = CARTESIAN_POINT ( 'NONE',  ( 0.000000000000000000, -3.031088913245509886, 1.750000000000043077 ) ) ;
#3807 = CARTESIAN_POINT ( 'NONE',  ( -2.521662442312483599, 27.57191497400664204, 15.12280841526694353 ) ) ;
#3808 = CARTESIAN_POINT ( 'NONE',  ( -1.814555661125937247, 28.27902175519318817, 15.12280841526694353 ) ) ;
#3809 = CIRCLE ( 'NONE', #778, 3.499999999999999556 ) ;
#3810 = DIRECTION ( 'NONE',  ( 0.000000000000000000, 0.4999999999999993339, -0.8660254037844390407 ) ) ;
#3811 = CARTESIAN_POINT ( 'NONE',  ( -26.48978331829069788, 57.12923484186614331, -6.938092349935781833 ) ) ;
#3812 = CIRCLE ( 'NONE', #10896, 2.149999999999992362 ) ;
#3813 = CARTESIAN_POINT ( 'NONE',  ( -25.98076211353311393, 53.43749999808803608, -3.000000000000132339 ) ) ;
#3814 = CARTESIAN_POINT ( 'NONE',  ( -25.98076211353311393, 49.49999999999986500, -5.000000000000103029 ) ) ;
#3815 = CARTESIAN_POINT ( 'NONE',  ( -25.17020516978313083, 51.41041666571061342, -6.403925809002825709 ) ) ;
#3816 = CARTESIAN_POINT ( 'NONE',  ( 25.98076211353311749, 56.49999999999984368, 10.00000000000000178 ) ) ;
#3817 = FACE_OUTER_BOUND ( 'NONE', #4191, .T. ) ;
#3818 = AXIS2_PLACEMENT_3D ( 'NONE', #1665, #5063, #5526 ) ;
#3819 = VERTEX_POINT ( 'NONE', #7403 ) ;
#3820 = AXIS2_PLACEMENT_3D ( 'NONE', #8689, #8737, #4523 ) ;
#3821 = AXIS2_PLACEMENT_3D ( 'NONE', #6130, #1858, #10357 ) ;
#3822 = CIRCLE ( 'NONE', #8079, 2.149999999999995470 ) ;
#3823 = DIRECTION ( 'NONE',  ( 0.000000000000000000, 0.000000000000000000, 1.000000000000000000 ) ) ;
#3824 = EDGE_CURVE ( 'NONE', #6934, #4635, #3304, .T. ) ;
#3825 = ORIENTED_EDGE ( 'NONE', *, *, #2409, .F. ) ;
#3826 = LINE ( 'NONE', #2161, #2394 ) ;
#3827 = AXIS2_PLACEMENT_3D ( 'NONE', #10010, #5787, #9172 ) ;
#3828 = CARTESIAN_POINT ( 'NONE',  ( -26.79131905728310059, 49.95208333237728482, -6.403925809002825709 ) ) ;
#3829 = VECTOR ( 'NONE', #7761, 1000.000000000000114 ) ;
#3830 = CARTESIAN_POINT ( 'NONE',  ( 16.06885556321644160, 18.88089190506775594, 11.22291988893967840 ) ) ;
#3831 = VERTEX_POINT ( 'NONE', #3355 ) ;
#3832 = ADVANCED_FACE ( 'NONE', ( #2468 ), #1684, .F. ) ;
#3833 = CARTESIAN_POINT ( 'NONE',  ( -24.35964822603314772, 55.43541666571061199, -4.064049460664953983 ) ) ;
#3834 = ORIENTED_EDGE ( 'NONE', *, *, #6155, .F. ) ;
#3835 = CARTESIAN_POINT ( 'NONE',  ( 2.371692252312040949E-17, -0.3416191432522661664, 3.499999999999999112 ) ) ;
#3836 = ORIENTED_EDGE ( 'NONE', *, *, #9273, .F. ) ;
#3837 = CARTESIAN_POINT ( 'NONE',  ( 4.553649124439118623E-15, 27.49999999999999289, 14.28125000000000355 ) ) ;
#3838 =( LENGTH_UNIT ( ) NAMED_UNIT ( * ) SI_UNIT ( .MILLI., .METRE. ) );
#3839 = ORIENTED_EDGE ( 'NONE', *, *, #1853, .T. ) ;
#3840 = CARTESIAN_POINT ( 'NONE',  ( 19.52895938645546536, 19.09041019265748673, 10.95195840513859586 ) ) ;
#3841 =( LENGTH_UNIT ( ) NAMED_UNIT ( * ) SI_UNIT ( .MILLI., .METRE. ) );
#3842 = CARTESIAN_POINT ( 'NONE',  ( 2.725741868436127202, -3.045094352033990148, -3.220599429844051453 ) ) ;
#3843 = CARTESIAN_POINT ( 'NONE',  ( 19.71976556488538534, 21.01616815698335827, 13.00425721518307753 ) ) ;
#3844 = EDGE_CURVE ( 'NONE', #5854, #2292, #10358, .T. ) ;
#3845 = AXIS2_PLACEMENT_3D ( 'NONE', #2754, #9521, #4481 ) ;
#3846 = DIRECTION ( 'NONE',  ( 4.312387734422005941E-17, -0.7071067811865500152, 0.7071067811865451302 ) ) ;
#3847 = CARTESIAN_POINT ( 'NONE',  ( -2.855764796983342624, 2.970025579236414082, -0.09382832055445475272 ) ) ;
#3848 = FACE_OUTER_BOUND ( 'NONE', #4967, .T. ) ;
#3849 = PRODUCT_DEFINITION_SHAPE ( 'NONE', 'NONE',  #6396 ) ;
#3850 = ORIENTED_EDGE ( 'NONE', *, *, #7228, .T. ) ;
#3851 = ORIENTED_EDGE ( 'NONE', *, *, #4672, .F. ) ;
#3852 = ADVANCED_FACE ( 'NONE', ( #9178 ), #2065, .T. ) ;
#3853 = CARTESIAN_POINT ( 'NONE',  ( 23.04535143233503192, 19.92821688535955360, 12.00579112326941988 ) ) ;
#3854 = CARTESIAN_POINT ( 'NONE',  ( -23.98076211353314235, 52.24166666666652503, -3.845299461620867554 ) ) ;
#3855 = VECTOR ( 'NONE', #3132, 1000.000000000000000 ) ;
#3856 = CARTESIAN_POINT ( 'NONE',  ( 0.03019833794501310467, 0.6882444255504208686, 3.500000000000000444 ) ) ;
#3857 = DIRECTION ( 'NONE',  ( 1.000000000000000000, 0.000000000000000000, 0.000000000000000000 ) ) ;
#3858 = FACE_BOUND ( 'NONE', #8467, .T. ) ;
#3859 = CARTESIAN_POINT ( 'NONE',  ( 2.474873734152922111, 27.52512626584708144, 14.43750000000000178 ) ) ;
#3860 = DIRECTION ( 'NONE',  ( 0.000000000000000000, 0.000000000000000000, 1.000000000000000000 ) ) ;
#3861 = UNCERTAINTY_MEASURE_WITH_UNIT (LENGTH_MEASURE( 1.000000000000000082E-05 ), #4997, 'distance_accuracy_value', 'NONE');
#3862 = ADVANCED_FACE ( 'NONE', ( #3239 ), #3183, .T. ) ;
#3863 = VERTEX_POINT ( 'NONE', #4857 ) ;
#3864 = SURFACE_STYLE_USAGE ( .BOTH. , #7982 ) ;
#3865 = AXIS2_PLACEMENT_3D ( 'NONE', #8053, #9666, #8777 ) ;
#3866 = AXIS2_PLACEMENT_3D ( 'NONE', #7073, #4574, #1911 ) ;
#3867 = CARTESIAN_POINT ( 'NONE',  ( -1.720978244806810498, 31.81455566112594013, 17.31030841526694175 ) ) ;
#3868 = DIRECTION ( 'NONE',  ( 1.000000000000000000, 0.000000000000000000, 0.000000000000000000 ) ) ;
#3869 = DIRECTION ( 'NONE',  ( 0.000000000000000000, 0.000000000000000000, 1.000000000000000000 ) ) ;
#3870 = DIRECTION ( 'NONE',  ( -0.000000000000000000, -0.000000000000000000, -1.000000000000000000 ) ) ;
#3871 = CARTESIAN_POINT ( 'NONE',  ( -24.98076211353312814, 51.71666666666652645, -6.732050807568954909 ) ) ;
#3872 = CARTESIAN_POINT ( 'NONE',  ( -25.17020516978313083, 53.51041666571060773, -6.403925809002825709 ) ) ;
#3873 = CARTESIAN_POINT ( 'NONE',  ( 0.000000000000000000, 0.000000000000000000, 1.650000000000000355 ) ) ;
#3874 = CIRCLE ( 'NONE', #9734, 0.2000000000000000944 ) ;
#3875 = ORIENTED_EDGE ( 'NONE', *, *, #358, .T. ) ;
#3876 = COLOUR_RGB ( '', 0.31764706, 0.68627451, 0.89019608) ;
#3877 = CARTESIAN_POINT ( 'NONE',  ( 0.000000000000000000, 0.000000000000000000, 0.000000000000000000 ) ) ;
#3878 = FACE_OUTER_BOUND ( 'NONE', #7752, .T. ) ;
#3879 = VERTEX_POINT ( 'NONE', #6679 ) ;
#3880 =( GEOMETRIC_REPRESENTATION_CONTEXT ( 3 ) GLOBAL_UNCERTAINTY_ASSIGNED_CONTEXT ( ( #515 ) ) GLOBAL_UNIT_ASSIGNED_CONTEXT ( ( #7040, #8589, #4098 ) ) REPRESENTATION_CONTEXT ( 'NONE', 'WORKASPACE' ) );
#3881 = DIRECTION ( 'NONE',  ( -0.000000000000000000, -0.000000000000000000, -1.000000000000000000 ) ) ;
#3882 = CARTESIAN_POINT ( 'NONE',  ( -24.35964822603314772, 50.47708333237728340, -5.935950539335252074 ) ) ;
#3883 = EDGE_CURVE ( 'NONE', #1907, #927, #5906, .T. ) ;
#3884 = CARTESIAN_POINT ( 'NONE',  ( 22.26413902940654665, 19.29239618210221607, 11.00732503135576401 ) ) ;
#3885 = VERTEX_POINT ( 'NONE', #7575 ) ;
#3886 = CARTESIAN_POINT ( 'NONE',  ( -25.98076211353311393, 53.08749999808803466, -7.000000000000072831 ) ) ;
#3887 = EDGE_LOOP ( 'NONE', ( #9823, #655, #4584 ) ) ;
#3888 = FACE_OUTER_BOUND ( 'NONE', #3934, .T. ) ;
#3889 = ORIENTED_EDGE ( 'NONE', *, *, #1459, .T. ) ;
#3890 = DIRECTION ( 'NONE',  ( 1.000000000000000000, 0.000000000000000000, 0.000000000000000000 ) ) ;
#3891 = SURFACE_STYLE_FILL_AREA ( #1443 ) ;
#3892 = ORIENTED_EDGE ( 'NONE', *, *, #4458, .T. ) ;
#3893 = CARTESIAN_POINT ( 'NONE',  ( 16.67998965505631404, 16.85551971246726310, 11.09929001438087148 ) ) ;
#3894 =( LENGTH_UNIT ( ) NAMED_UNIT ( * ) SI_UNIT ( .MILLI., .METRE. ) );
#3895 = ADVANCED_FACE ( 'NONE', ( #10964 ), #9289, .F. ) ;
#3896 = CARTESIAN_POINT ( 'NONE',  ( 0.000000000000000000, 0.000000000000000000, -3.499999999999999556 ) ) ;
#3897 = EDGE_CURVE ( 'NONE', #4107, #8160, #5969, .T. ) ;
#3898 = CARTESIAN_POINT ( 'NONE',  ( 23.02513694122459498, 21.97618599832468433, 13.00425721518307753 ) ) ;
#3899 = CARTESIAN_POINT ( 'NONE',  ( -26.98076211353309972, 52.44583333142136894, -6.732050807568954909 ) ) ;
#3900 = CARTESIAN_POINT ( 'NONE',  ( -27.98076211353308551, 53.40833333333319644, -3.845299461620869330 ) ) ;
#3901 = CARTESIAN_POINT ( 'NONE',  ( -27.98076211353308551, 51.16249999808803750, -5.000000000000103029 ) ) ;
#3902 = ORIENTED_EDGE ( 'NONE', *, *, #6379, .T. ) ;
#3903 = VERTEX_POINT ( 'NONE', #8231 ) ;
#3904 = CARTESIAN_POINT ( 'NONE',  ( 17.69587633286529282, 17.26453111358909354, 13.07531547515800874 ) ) ;
#3905 = EDGE_CURVE ( 'NONE', #3831, #1717, #6848, .T. ) ;
#3906 = CARTESIAN_POINT ( 'NONE',  ( 34.99999999999999289, -3.999999999999993339, -7.149999999999987921 ) ) ;
#3907 = CARTESIAN_POINT ( 'NONE',  ( 0.000000000000000000, 0.000000000000000000, 0.000000000000000000 ) ) ;
#3908 = CARTESIAN_POINT ( 'NONE',  ( 29.49999999999999645, 0.5000000000000163203, 10.00000000000000888 ) ) ;
#3909 = EDGE_CURVE ( 'NONE', #2599, #10270, #481, .T. ) ;
#3910 = ADVANCED_FACE ( 'NONE', ( #1516 ), #2405, .F. ) ;
#3911 = SURFACE_STYLE_FILL_AREA ( #5837 ) ;
#3912 = CARTESIAN_POINT ( 'NONE',  ( 0.06616922564517879746, 26.50000000000000000, 13.28344158473306713 ) ) ;
#3913 = FACE_OUTER_BOUND ( 'NONE', #1607, .T. ) ;
#3914 = CARTESIAN_POINT ( 'NONE',  ( -1.219727444046192735E-16, 2.000000000000000000, 0.000000000000000000 ) ) ;
#3915 = CARTESIAN_POINT ( 'NONE',  ( 21.21106610644839208, 56.49999999999984368, 14.50000000000000000 ) ) ;
#3916 = CARTESIAN_POINT ( 'NONE',  ( 0.9693646802875698354, 27.47259180932603684, 15.35718341526694530 ) ) ;
#3917 = CARTESIAN_POINT ( 'NONE',  ( -3.049318610115481714E-16, 5.000000000000000000, -5.500000000000000000 ) ) ;
#3918 = DIRECTION ( 'NONE',  ( 0.000000000000000000, 0.000000000000000000, -1.000000000000000000 ) ) ;
#3919 = CYLINDRICAL_SURFACE ( 'NONE', #10740, 2.649999999999991029 ) ;
#3920 = LINE ( 'NONE', #7147, #7041 ) ;
#3921 = CARTESIAN_POINT ( 'NONE',  ( -25.98076211353311393, 49.89374999904395480, -6.871901078670400231 ) ) ;
#3922 = CARTESIAN_POINT ( 'NONE',  ( 3.199999999999999734, 0.000000000000000000, -3.499999999999999556 ) ) ;
#3923 = CARTESIAN_POINT ( 'NONE',  ( -26.51666049839535688, 55.30626073911682994, -7.000000000000071942 ) ) ;
#3924 = AXIS2_PLACEMENT_3D ( 'NONE', #2465, #5847, #9230 ) ;
#3925 = ORIENTED_EDGE ( 'NONE', *, *, #603, .T. ) ;
#3926 = DIRECTION ( 'NONE',  ( 0.000000000000000000, 0.000000000000000000, -1.000000000000000000 ) ) ;
#3927 = CARTESIAN_POINT ( 'NONE',  ( 1.767766952966372429, 31.76776695296637598, 13.50000000000000355 ) ) ;
#3928 = ADVANCED_FACE ( 'NONE', ( #6790, #5962 ), #899, .F. ) ;
#3929 = EDGE_LOOP ( 'NONE', ( #5381, #4219, #2726, #343 ) ) ;
#3930 = DIRECTION ( 'NONE',  ( -1.000000000000000000, 0.000000000000000000, 0.000000000000000000 ) ) ;
#3931 = VECTOR ( 'NONE', #5738, 1000.000000000000227 ) ;
#3932 = CARTESIAN_POINT ( 'NONE',  ( -27.60187600103308725, 52.92708333237727913, -4.064049460664955760 ) ) ;
#3933 = CARTESIAN_POINT ( 'NONE',  ( 22.44007493706583745, 19.34731747087121434, 12.00579112326928133 ) ) ;
#3934 = EDGE_LOOP ( 'NONE', ( #5829, #3512, #332, #4799 ) ) ;
#3935 = CARTESIAN_POINT ( 'NONE',  ( 3.170065989602867784, -2.688325911136562052, -2.343682934607623558 ) ) ;
#3936 = EDGE_LOOP ( 'NONE', ( #10469, #8350, #7432, #128 ) ) ;
#3937 = ORIENTED_EDGE ( 'NONE', *, *, #4069, .T. ) ;
#3938 = CARTESIAN_POINT ( 'NONE',  ( -3.510273485745307287, -2.827716139362669967, -3.610536846335890004 ) ) ;
#3939 = ORIENTED_EDGE ( 'NONE', *, *, #2559, .T. ) ;
#3940 = DIRECTION ( 'NONE',  ( 0.000000000000000000, -1.000000000000000000, 0.000000000000000000 ) ) ;
#3941 = ORIENTED_EDGE ( 'NONE', *, *, #2539, .T. ) ;
#3942 = CARTESIAN_POINT ( 'NONE',  ( 19.46525898981753855, 16.20608772750926718, 10.95621100456342312 ) ) ;
#3943 =( LENGTH_UNIT ( ) NAMED_UNIT ( * ) SI_UNIT ( .MILLI., .METRE. ) );
#3944 = AXIS2_PLACEMENT_3D ( 'NONE', #9541, #2834, #6316 ) ;
#3945 = CARTESIAN_POINT ( 'NONE',  ( 4.000000000000000000, 2.309401076758497151, -3.433295621305379353 ) ) ;
#3946 = CARTESIAN_POINT ( 'NONE',  ( 22.45649315185626094, 23.58010107951569623, 12.94889058896590583 ) ) ;
#3947 = CARTESIAN_POINT ( 'NONE',  ( -23.98076211353314235, 51.45416666475470180, -3.845299461620867554 ) ) ;
#3948 = AXIS2_PLACEMENT_3D ( 'NONE', #6167, #8726, #7896 ) ;
#3949 = DIRECTION ( 'NONE',  ( -1.000000000000000000, 0.000000000000000000, 0.000000000000000000 ) ) ;
#3950 = LINE ( 'NONE', #6602, #9899 ) ;
#3951 = ORIENTED_EDGE ( 'NONE', *, *, #2893, .T. ) ;
#3952 = EDGE_LOOP ( 'NONE', ( #4222, #3108, #8056, #303 ) ) ;
#3953 = CARTESIAN_POINT ( 'NONE',  ( 22.82387490247590733, 19.65457484615246386, 12.00579112326941988 ) ) ;
#3954 = DIRECTION ( 'NONE',  ( 1.000000000000000000, 0.000000000000000000, 0.000000000000000000 ) ) ;
#3955 = CARTESIAN_POINT ( 'NONE',  ( -1.240299975428134203E-15, -4.736529461165891242, -3.681130640444276292 ) ) ;
#3956 = DIRECTION ( 'NONE',  ( 1.000000000000000000, 0.000000000000000000, 0.000000000000000000 ) ) ;
#3957 = CARTESIAN_POINT ( 'NONE',  ( -1.383578242660655100, 26.47259180932604039, 14.45531658473306535 ) ) ;
#3958 = CARTESIAN_POINT ( 'NONE',  ( 24.49999999999999289, -1.232050807568863426, -4.999999999999992006 ) ) ;
#3959 = EDGE_CURVE ( 'NONE', #10270, #8937, #5142, .T. ) ;
#3960 = FACE_OUTER_BOUND ( 'NONE', #4066, .T. ) ;
#3961 = FACE_OUTER_BOUND ( 'NONE', #9048, .T. ) ;
#3962 = EDGE_CURVE ( 'NONE', #1907, #7434, #2960, .T. ) ;
#3963 = ORIENTED_EDGE ( 'NONE', *, *, #10153, .T. ) ;
#3964 = CARTESIAN_POINT ( 'NONE',  ( -1.383578242660661983, 33.52740819067396671, 14.73218341526694175 ) ) ;
#3965 = FACE_OUTER_BOUND ( 'NONE', #8221, .T. ) ;
#3966 = DIRECTION ( 'NONE',  ( 0.000000000000000000, 0.000000000000000000, -1.000000000000000000 ) ) ;
#3967 = FACE_OUTER_BOUND ( 'NONE', #2410, .T. ) ;
#3968 = CARTESIAN_POINT ( 'NONE',  ( -27.98076211353308551, 51.19166666666652787, -6.154700538379338504 ) ) ;
#3969 = CARTESIAN_POINT ( 'NONE',  ( -25.17020516978313083, 50.30208333237728624, -3.596074190997380349 ) ) ;
#3970 = AXIS2_PLACEMENT_3D ( 'NONE', #9320, #929, #2493 ) ;
#3971 = CARTESIAN_POINT ( 'NONE',  ( 0.000000000000000000, 0.8865213383406680414, -1.535500000000000975 ) ) ;
#3972 = CARTESIAN_POINT ( 'NONE',  ( 2.000000000000000000, -1.502314598737159426E-15, -1.535500000000000087 ) ) ;
#3973 = ORIENTED_EDGE ( 'NONE', *, *, #6831, .T. ) ;
#3974 = CARTESIAN_POINT ( 'NONE',  ( -3.500000000000003109, 29.99999999999999645, 15.21875000000000355 ) ) ;
#3975 = COLOUR_RGB ( '', 0.66274510, 0.83137255, 0.94901961) ;
#3976 = DIRECTION ( 'NONE',  ( 0.000000000000000000, 1.000000000000000000, 0.000000000000000000 ) ) ;
#3977 = AXIS2_PLACEMENT_3D ( 'NONE', #4394, #6716, #7781 ) ;
#3978 = DIRECTION ( 'NONE',  ( 0.000000000000000000, 0.000000000000000000, 1.000000000000000000 ) ) ;
#3979 = CARTESIAN_POINT ( 'NONE',  ( -25.98076211353310683, 55.14374999904394059, -3.128098921329806714 ) ) ;
#3980 = CIRCLE ( 'NONE', #10384, 7.500000000000000000 ) ;
#3981 = CARTESIAN_POINT ( 'NONE',  ( 23.33980466280999977, 20.94445964013513617, 12.00579112326902909 ) ) ;
#3982 = CARTESIAN_POINT ( 'NONE',  ( -25.98076211353311393, 50.02499999999986358, -2.690598923241634743 ) ) ;
#3983 = AXIS2_PLACEMENT_3D ( 'NONE', #3427, #2657, #3541 ) ;
#3984 = ORIENTED_EDGE ( 'NONE', *, *, #5002, .T. ) ;
#3985 = CARTESIAN_POINT ( 'NONE',  ( 29.49999999999999645, -9.999999999999998224, -12.49999999999999822 ) ) ;
#3986 = ORIENTED_EDGE ( 'NONE', *, *, #9616, .T. ) ;
#3988 = VERTEX_POINT ( 'NONE', #10697 ) ;
#3987 = EDGE_CURVE ( 'NONE', #9988, #3885, #9512, .T. ) ;
#3989 = FACE_BOUND ( 'NONE', #8269, .T. ) ;
#3990 = VERTEX_POINT ( 'NONE', #2198 ) ;
#3991 = CARTESIAN_POINT ( 'NONE',  ( -1.035533905932742638, 32.50000000000000000, 16.23437500000000355 ) ) ;
#3992 = SHAPE_REPRESENTATION_RELATIONSHIP ( 'NONE' , 'NONE' ,  #6402, #10767 ) ;
#3993 = VECTOR ( 'NONE', #6997, 1000.000000000000227 ) ;
#3994 = EDGE_LOOP ( 'NONE', ( #6071, #6195, #7981, #7395 ) ) ;
#3995 = CARTESIAN_POINT ( 'NONE',  ( 21.87443830563928415, 19.02131736398618855, 11.00732503135576401 ) ) ;
#3996 = VECTOR ( 'NONE', #10258, 1000.000000000000000 ) ;
#3997 = CARTESIAN_POINT ( 'NONE',  ( 3.522875095019493141, -2.820352903225631369, -3.598441714920572299 ) ) ;
#3998 = CARTESIAN_POINT ( 'NONE',  ( 18.94130700685887447, 16.00034706198404066, 11.96718634320919250 ) ) ;
#3999 = VECTOR ( 'NONE', #4815, 1000.000000000000000 ) ;
#4000 = CARTESIAN_POINT ( 'NONE',  ( -27.98076211353308551, 50.52083333142136468, -3.845299461620869330 ) ) ;
#4001 = CIRCLE ( 'NONE', #5090, 3.499999999999997780 ) ;
#4002 = CARTESIAN_POINT ( 'NONE',  ( -27.98076211353308551, 53.29166666666652930, -6.154700538379338504 ) ) ;
#4003 = DIRECTION ( 'NONE',  ( 0.000000000000000000, 0.000000000000000000, 1.000000000000000000 ) ) ;
#4004 = B_SPLINE_CURVE_WITH_KNOTS ( 'NONE', 1,
 ( #10033, #4030 ),
 .UNSPECIFIED., .F., .F.,
 ( 2, 2 ),
 ( 0.000000000000000000, 1.000000000000000000 ),
 .UNSPECIFIED. ) ;
#4005 = VERTEX_POINT ( 'NONE', #6373 ) ;
#4006 = CARTESIAN_POINT ( 'NONE',  ( 3.472591809326051937, 28.48408330604899419, 15.51343341526694353 ) ) ;
#4007 = VERTEX_POINT ( 'NONE', #8821 ) ;
#4008 =( REPRESENTATION_RELATIONSHIP ('NONE','NONE', #7540, #3016 ) REPRESENTATION_RELATIONSHIP_WITH_TRANSFORMATION ( #10500 )SHAPE_REPRESENTATION_RELATIONSHIP( ) );
#4009 = CARTESIAN_POINT ( 'NONE',  ( 21.05771646464872404, 22.57981893131178452, 12.00579112326941988 ) ) ;
#4010 = AXIS2_PLACEMENT_3D ( 'NONE', #4604, #5171, #6824 ) ;
#4011 = CARTESIAN_POINT ( 'NONE',  ( -23.98076211353314235, 52.29999999999986215, -5.000000000000103029 ) ) ;
#4012 = CARTESIAN_POINT ( 'NONE',  ( 34.66939513580730647, 4.803384628401709655, 2.499999999999999556 ) ) ;
#4013 = DIRECTION ( 'NONE',  ( -0.000000000000000000, -0.000000000000000000, 1.000000000000000000 ) ) ;
#4014 = ADVANCED_FACE ( 'NONE', ( #9646 ), #6467, .T. ) ;
#4015 = CARTESIAN_POINT ( 'NONE',  ( -3.527408190673960053, 31.38357824266065066, 12.89281658473306535 ) ) ;
#4016 = DIRECTION ( 'NONE',  ( 1.224646799147353207E-16, 1.000000000000000000, 0.000000000000000000 ) ) ;
#4017 = EDGE_LOOP ( 'NONE', ( #4439, #5341, #5379 ) ) ;
#4018 = CARTESIAN_POINT ( 'NONE',  ( 24.99999259214812142, 30.01924558493218598, 2.500000000000000000 ) ) ;
#4019 = ORIENTED_EDGE ( 'NONE', *, *, #9675, .T. ) ;
#4020 = CARTESIAN_POINT ( 'NONE',  ( -0.9693646802875689472, 32.52740819067395961, 14.73218341526694175 ) ) ;
#4021 = DIRECTION ( 'NONE',  ( 0.000000000000000000, 0.000000000000000000, -1.000000000000000000 ) ) ;
#4022 = AXIS2_PLACEMENT_3D ( 'NONE', #6766, #1661, #10110 ) ;
#4023 = CARTESIAN_POINT ( 'NONE',  ( 17.45361707773674809, 17.49611573659335662, 12.09524845743996657 ) ) ;
#4024 = DIRECTION ( 'NONE',  ( 0.000000000000000000, 0.000000000000000000, 1.000000000000000000 ) ) ;
#4025 = EDGE_CURVE ( 'NONE', #10232, #6011, #1627, .T. ) ;
#4026 = CARTESIAN_POINT ( 'NONE',  ( 3.999999999999999112, -1.539600717839012978, -3.300726591567080703 ) ) ;
#4027 = CARTESIAN_POINT ( 'NONE',  ( -24.35964822603314417, 49.71874999904395054, -5.000000000000103029 ) ) ;
#4028 = EDGE_CURVE ( 'NONE', #3729, #10824, #3920, .T. ) ;
#4029 = CARTESIAN_POINT ( 'NONE',  ( 2.500000000000000000, -1.178949249685218303, -2.041999999999998039 ) ) ;
#4030 = CARTESIAN_POINT ( 'NONE',  ( -24.35964822603314417, 49.71874999904395054, -5.000000000000103029 ) ) ;
#4031 = ORIENTED_EDGE ( 'NONE', *, *, #2433, .F. ) ;
#4032 = VECTOR ( 'NONE', #10535, 1000.000000000000000 ) ;
#4033 = AXIS2_PLACEMENT_3D ( 'NONE', #2231, #7227, #10624 ) ;
#4034 = CARTESIAN_POINT ( 'NONE',  ( 29.50000000000000711, 1.387778780781445676E-14, 17.49999999999999645 ) ) ;
#4035 = CYLINDRICAL_SURFACE ( 'NONE', #4341, 1.999999999999971356 ) ;
#4036 = B_SPLINE_CURVE_WITH_KNOTS ( 'NONE', 3,
 ( #5587, #10592, #8972, #3806 ),
 .UNSPECIFIED., .F., .F.,
 ( 4, 4 ),
 ( 2.380739282168429972E-07, 0.002044882221487562268 ),
 .UNSPECIFIED. ) ;
#4037 = FACE_OUTER_BOUND ( 'NONE', #2439, .T. ) ;
#4038 = EDGE_CURVE ( 'NONE', #4616, #4976, #4379, .T. ) ;
#4039 = CARTESIAN_POINT ( 'NONE',  ( -25.17020516978313083, 52.40208333237728766, -3.596074190997380349 ) ) ;
#4040 = VECTOR ( 'NONE', #5781, 1000.000000000000000 ) ;
#4041 =( GEOMETRIC_REPRESENTATION_CONTEXT ( 3 ) GLOBAL_UNCERTAINTY_ASSIGNED_CONTEXT ( ( #2529 ) ) GLOBAL_UNIT_ASSIGNED_CONTEXT ( ( #1114, #6063, #4469 ) ) REPRESENTATION_CONTEXT ( 'NONE', 'WORKASPACE' ) );
#4042 = MECHANICAL_DESIGN_GEOMETRIC_PRESENTATION_REPRESENTATION (  '', ( #10621 ), #5476 ) ;
#4043 = CARTESIAN_POINT ( 'NONE',  ( 21.51635413324704160, 18.70478684647606826, 12.00579112326941988 ) ) ;
#4044 = CARTESIAN_POINT ( 'NONE',  ( -25.17020516978313083, 53.10208333237728340, -3.596074190997380349 ) ) ;
#4045 = VERTEX_POINT ( 'NONE', #6314 ) ;
#4046 = EDGE_CURVE ( 'NONE', #6011, #491, #4325, .T. ) ;
#4047 = ADVANCED_FACE ( 'NONE', ( #9813 ), #6170, .F. ) ;
#4048 = CARTESIAN_POINT ( 'NONE',  ( -26.79131905728310059, 55.72708333237728340, -6.403925809002825709 ) ) ;
#4049 = ORIENTED_EDGE ( 'NONE', *, *, #624, .T. ) ;
#4050 = ORIENTED_EDGE ( 'NONE', *, *, #7335, .T. ) ;
#4051 = CARTESIAN_POINT ( 'NONE',  ( -26.25045812061784289, 13.49999999999941913, -9.500000000000000000 ) ) ;
#4052 = ORIENTED_EDGE ( 'NONE', *, *, #6268, .F. ) ;
#4053 = AXIS2_PLACEMENT_3D ( 'NONE', #487, #9775, #2166 ) ;
#4054 = CARTESIAN_POINT ( 'NONE',  ( -25.98076211353311038, 61.49999999999985789, -5.000000000000102141 ) ) ;
#4055 = SHAPE_REPRESENTATION_RELATIONSHIP ( 'NONE' , 'NONE' ,  #7975, #4816 ) ;
#4056 = EDGE_LOOP ( 'NONE', ( #1230, #9407, #4490, #6501 ) ) ;
#4057 = AXIS2_PLACEMENT_3D ( 'NONE', #7619, #2141, #6162 ) ;
#4058 = CARTESIAN_POINT ( 'NONE',  ( 17.54702143963720928, 17.40274154661815587, 11.08429399133878057 ) ) ;
#4059 = FILL_AREA_STYLE ('',( #7440 ) ) ;
#4060 = CARTESIAN_POINT ( 'NONE',  ( -4.000000000000000000, 2.309401076758498483, -0.4999999999999927280 ) ) ;
#4061 = CARTESIAN_POINT ( 'NONE',  ( 4.101954839143060028, 2.368264730582927857, -3.681130640444267854 ) ) ;
#4062 = CARTESIAN_POINT ( 'NONE',  ( 17.82816014985957054, 16.05830732944317418, 13.01541525850460168 ) ) ;
#4063 = CARTESIAN_POINT ( 'NONE',  ( -24.98076211353312814, 50.22916666475470038, -6.732050807568954909 ) ) ;
#4064 = FACE_OUTER_BOUND ( 'NONE', #10247, .T. ) ;
#4065 = CARTESIAN_POINT ( 'NONE',  ( 20.23853826540680600, 19.71164639310234534, 12.00579112326941988 ) ) ;
#4066 = EDGE_LOOP ( 'NONE', ( #1224, #891, #8538, #592, #4500, #3107, #3501, #9461 ) ) ;
#4067 = CARTESIAN_POINT ( 'NONE',  ( 1.515916693951008254, 33.47259180932604750, 14.57593341526694175 ) ) ;
#4068 = EDGE_LOOP ( 'NONE', ( #4858, #9181, #28, #7897 ) ) ;
#4069 = EDGE_CURVE ( 'NONE', #4861, #8872, #10222, .T. ) ;
#4070 = CARTESIAN_POINT ( 'NONE',  ( 18.97799213218983994, 15.95698123192398477, 12.96557279687576525 ) ) ;
#4071 = LINE ( 'NONE', #4803, #2948 ) ;
#4072 = CARTESIAN_POINT ( 'NONE',  ( 24.49999999999998934, -3.999999999999983569, 10.00000000000000888 ) ) ;
#4073 = CARTESIAN_POINT ( 'NONE',  ( 1.734723475976807094E-15, 4.618802153517012954, -0.4999999999999995559 ) ) ;
#4074 = CARTESIAN_POINT ( 'NONE',  ( 3.500000000000003997, 30.06616922564517580, 13.59594158473306358 ) ) ;
#4075 = CARTESIAN_POINT ( 'NONE',  ( -25.44486372867087454, 51.36876073720500102, -3.000000000000132339 ) ) ;
#4076 = ORIENTED_EDGE ( 'NONE', *, *, #8256, .F. ) ;
#4077 = DIRECTION ( 'NONE',  ( -1.000000000000000000, 0.000000000000000000, 0.000000000000000000 ) ) ;
#4078 = ORIENTED_EDGE ( 'NONE', *, *, #4312, .F. ) ;
#4079 = VERTEX_POINT ( 'NONE', #5032 ) ;
#4080 = DIRECTION ( 'NONE',  ( -1.000000000000000000, -0.000000000000000000, -0.000000000000000000 ) ) ;
#4081 = CYLINDRICAL_SURFACE ( 'NONE', #2969, 2.500000000000000444 ) ;
#4082 = EDGE_CURVE ( 'NONE', #3312, #1951, #8529, .T. ) ;
#4083 = CARTESIAN_POINT ( 'NONE',  ( 17.36588923991300604, 17.58385822839129986, 12.10347664333366247 ) ) ;
#4084 = DIRECTION ( 'NONE',  ( -1.000000000000000000, 0.000000000000000000, 0.000000000000000000 ) ) ;
#4085 = CARTESIAN_POINT ( 'NONE',  ( 34.94281041931230902, 2.000000000000002220, 5.102623512424888652 ) ) ;
#4086 = CARTESIAN_POINT ( 'NONE',  ( -26.79131905728310059, 55.26041666571061484, -3.596074190997381237 ) ) ;
#4087 = CARTESIAN_POINT ( 'NONE',  ( 1.734723475976807094E-15, 4.618802153517012954, -0.4999999999999995559 ) ) ;
#4088 = CARTESIAN_POINT ( 'NONE',  ( 4.204115023516791005, -1.660442669500199919, -3.602151381774560068 ) ) ;
#4089 = ORIENTED_EDGE ( 'NONE', *, *, #7793, .T. ) ;
#4090 = DIRECTION ( 'NONE',  ( -1.000000000000000000, -6.098637220230963674E-17, 0.000000000000000000 ) ) ;
#4091 = CARTESIAN_POINT ( 'NONE',  ( 25.49999999999999645, -3.999999999999986233, -4.999999999999992006 ) ) ;
#4092 = CARTESIAN_POINT ( 'NONE',  ( -24.35964822603314772, 51.23541666571061626, -4.064049460664953983 ) ) ;
#4093 = CARTESIAN_POINT ( 'NONE',  ( -25.98076211353310683, 53.74374999904394912, -3.128098921329806714 ) ) ;
#4094 = CIRCLE ( 'NONE', #2692, 1.999999999999971356 ) ;
#4095 = CARTESIAN_POINT ( 'NONE',  ( 21.25655365073496839, 18.52406763439849513, 12.00579112326941988 ) ) ;
#4096 = CARTESIAN_POINT ( 'NONE',  ( -24.98076211353312814, 51.01666666666653072, -6.732050807568954909 ) ) ;
#4097 = ORIENTED_EDGE ( 'NONE', *, *, #3168, .F. ) ;
#4098 =( NAMED_UNIT ( * ) SI_UNIT ( $, .STERADIAN. ) SOLID_ANGLE_UNIT ( ) );
#4099 = EDGE_CURVE ( 'NONE', #8106, #8932, #1219, .T. ) ;
#4100 = ORIENTED_EDGE ( 'NONE', *, *, #9474, .F. ) ;
#4101 = ORIENTED_EDGE ( 'NONE', *, *, #421, .F. ) ;
#4102 = CARTESIAN_POINT ( 'NONE',  ( 29.50000000000000711, 2.000000000000001776, 17.49999999999999645 ) ) ;
#4104 = ORIENTED_EDGE ( 'NONE', *, *, #10897, .T. ) ;
#4103 = EDGE_CURVE ( 'NONE', #3173, #3779, #10582, .T. ) ;
#4105 = CARTESIAN_POINT ( 'NONE',  ( -1.767766952966375094, 31.76776695296636888, 16.31250000000000355 ) ) ;
#4106 = VECTOR ( 'NONE', #5848, 1000.000000000000000 ) ;
#4107 = VERTEX_POINT ( 'NONE', #10854 ) ;
#4108 = CARTESIAN_POINT ( 'NONE',  ( 17.36588923991300604, 17.58385822839129986, 12.10347664333366247 ) ) ;
#4109 = CARTESIAN_POINT ( 'NONE',  ( 27.50000000000001066, -3.999999999999986233, -4.999999999999992006 ) ) ;
#4110 = CARTESIAN_POINT ( 'NONE',  ( 0.2949799022107380542, 0.000000000000000000, 1.615000000000000213 ) ) ;
#4111 = CARTESIAN_POINT ( 'NONE',  ( 19.44564476272491049, 19.01746825227115067, 12.94889058896590761 ) ) ;
#4112 = CARTESIAN_POINT ( 'NONE',  ( 34.99999999999999289, -9.999999999999998224, -10.50000000000000355 ) ) ;
#4113 = CARTESIAN_POINT ( 'NONE',  ( -25.98076211353311393, 50.63749999808803182, -2.690598923241634743 ) ) ;
#4114 = CARTESIAN_POINT ( 'NONE',  ( 0.000000000000000000, 0.000000000000000000, 0.000000000000000000 ) ) ;
#4115 = DIRECTION ( 'NONE',  ( 0.000000000000000000, 0.4999999999999991118, -0.8660254037844390407 ) ) ;
#4116 = PRODUCT_DEFINITION_CONTEXT ( 'detailed design', #2307, 'design' ) ;
#4117 = ORIENTED_EDGE ( 'NONE', *, *, #5057, .T. ) ;
#4118 = CARTESIAN_POINT ( 'NONE',  ( 1.515916693951008254, 33.47259180932604750, 17.07593341526694530 ) ) ;
#4119 = ORIENTED_EDGE ( 'NONE', *, *, #8713, .F. ) ;
#4120 = CARTESIAN_POINT ( 'NONE',  ( 19.80390141066272491, 20.29503604781401904, 13.00425721518307753 ) ) ;
#4121 = CARTESIAN_POINT ( 'NONE',  ( 3.199999999999999734, 0.000000000000000000, 3.499999999999999556 ) ) ;
#4122 = CARTESIAN_POINT ( 'NONE',  ( 34.99999999999999289, -3.999999999999993339, 12.14999999999999503 ) ) ;
#4123 = AXIS2_PLACEMENT_3D ( 'NONE', #275, #3671, #7063 ) ;
#4124 = DIRECTION ( 'NONE',  ( 0.000000000000000000, 1.000000000000000000, 0.000000000000000000 ) ) ;
#4125 = CARTESIAN_POINT ( 'NONE',  ( -2.472591809326046608, 28.89829686842208289, 14.29906658473306358 ) ) ;
#4126 = ORIENTED_EDGE ( 'NONE', *, *, #8787, .T. ) ;
#4127 = CARTESIAN_POINT ( 'NONE',  ( 0.000000000000000000, 0.000000000000000000, 2.500000000000000000 ) ) ;
#4128 = ORIENTED_EDGE ( 'NONE', *, *, #8914, .T. ) ;
#4129 = ORIENTED_EDGE ( 'NONE', *, *, #5268, .T. ) ;
#4130 = EDGE_CURVE ( 'NONE', #3442, #9151, #5264, .T. ) ;
#4131 = CARTESIAN_POINT ( 'NONE',  ( 1.192664741381417277E-14, 3.202582148906763848, 1.452965002680410178 ) ) ;
#4132 = PLANE ( 'NONE',  #6148 ) ;
#4133 =( BOUNDED_CURVE ( )  B_SPLINE_CURVE ( 2, ( #5661, #642, #3199, #5707, #4991, #583, #8365, #2427, #7371, #3051, #8257, #7315, #9040, #10704, #6425, #10757, #6579, #9981, #9087, #1481, #5759, #9142, #1538, #4092, #9825, #4940, #8311, #694, #7480, #10868, #3257, #5816, #9201, #1593, #4143, #8991, #2210, #1382, #3489, #4267, #5216, #10263, #9372, #5104, #8421, #10152, #3433, #31, #88, #10205, #3316, #7710, #6871, #921, #6089, #2715, #1878, #2540, #6755, #2663, #1770, #6039, #5922, #9424, #9309, #5870, #6701, #10925, #2604, #5267, #8592, #1707, #9480, #5160, #7770, #10100, #7597, #2486, #6808, #10986, #8483, #3376, #6930, #866, #7655, #10320, #8542, #802, #8654, #1820, #5981, #9254, #4384, #4322, #1033, #978, #149, #3547, #4444, #1649, #5045, #4209, #2099, #1200, #2151 ),
 .UNSPECIFIED., .F., .F. ) 
 B_SPLINE_CURVE_WITH_KNOTS ( ( 3, 2, 2, 2, 2, 2, 2, 2, 2, 2, 2, 2, 2, 2, 2, 2, 2, 2, 2, 2, 2, 2, 2, 2, 2, 2, 2, 2, 2, 2, 2, 2, 2, 2, 2, 2, 2, 2, 2, 2, 2, 2, 2, 2, 2, 2, 2, 2, 2, 2, 2, 2, 3 ),
 ( 0.000000000000000000, 0.01944383300006776241, 0.03888766600013552482, 0.05833149900020328377, 0.07777533200027104965, 0.09721916500033880859, 0.1166629980004065675, 0.1361068310004743265, 0.1555506640005420993, 0.1749944970006098444, 0.1944383300006776172, 0.2138821630007453622, 0.2333259960008131351, 0.2527698290008809079, 0.2722136620009486530, 0.2916574950010164535, 0.3111013280010841986, 0.3305451610011519437, 0.3499889940012196887, 0.3694328270012874893, 0.3888766600013552344, 0.4083204930014230349, 0.4277643260014907245, 0.4472081590015585251, 0.4666519920016262701, 0.4860958250016940707, 0.5055396580017618158, 0.5249834910018296164, 0.5444273240018973059, 0.5638711570019651065, 0.5833149900020329071, 0.6027588230021005966, 0.6222026560021683972, 0.6416464890022361978, 0.6610903220023038873, 0.6805341550023716879, 0.6999779880024393774, 0.7194218210025072890, 0.7388656540025749786, 0.7583094870026426682, 0.7777533200027104687, 0.7971971530027782693, 0.8166409860028460699, 0.8360848190029137594, 0.8555286520029814490, 0.8749724850030493606, 0.8944163180031170501, 0.9138601510031848507, 0.9333039840032525403, 0.9527478170033203408, 0.9721916500033881414, 0.9916354830034558310, 1.000000000000000000 ),
 .UNSPECIFIED. ) 
 CURVE ( )  GEOMETRIC_REPRESENTATION_ITEM ( )  RATIONAL_B_SPLINE_CURVE ( ( 1.000000000000000000, 0.8660254037844387076, 1.000000000000000000, 0.8660254037844387076, 1.000000000000000000, 0.8660254037844387076, 1.000000000000000000, 0.8660254037844387076, 1.000000000000000000, 0.8660254037844387076, 1.000000000000000000, 0.8660254037844387076, 1.000000000000000000, 0.8660254037844387076, 1.000000000000000000, 0.8660254037844387076, 1.000000000000000000, 0.8660254037844387076, 1.000000000000000000, 0.8660254037844387076, 1.000000000000000000, 0.8660254037844387076, 1.000000000000000000, 0.8660254037844387076, 1.000000000000000000, 0.8660254037844387076, 1.000000000000000000, 0.8660254037844387076, 1.000000000000000000, 0.8660254037844387076, 1.000000000000000000, 0.8660254037844387076, 1.000000000000000000, 0.8660254037844387076, 1.000000000000000000, 0.8660254037844387076, 1.000000000000000000, 0.8660254037844387076, 1.000000000000000000, 0.8660254037844387076, 1.000000000000000000, 0.8660254037844387076, 1.000000000000000000, 0.8660254037844387076, 1.000000000000000000, 0.8660254037844387076, 1.000000000000000000, 0.8660254037844387076, 1.000000000000000000, 0.8660254037844387076, 1.000000000000000000, 0.8660254037844387076, 1.000000000000000000, 0.8660254037844387076, 1.000000000000000000, 0.8660254037844387076, 1.000000000000000000, 0.8660254037844387076, 1.000000000000000000, 0.8660254037844387076, 1.000000000000000000, 0.8660254037844387076, 1.000000000000000000, 0.8660254037844387076, 1.000000000000000000, 0.8660254037844387076, 1.000000000000000000, 0.8660254037844387076, 1.000000000000000000, 0.8660254037844387076, 1.000000000000000000, 0.8660254037844387076, 1.000000000000000000, 0.8660254037844387076, 1.000000000000000000, 0.8660254037844387076, 1.000000000000000000, 0.8660254037844387076, 1.000000000000000000, 0.8660254037844387076, 1.000000000000000000, 0.8660254037844387076, 1.000000000000000000, 0.8660254037844387076, 1.000000000000000000, 0.8660254037844387076, 1.000000000000000000, 0.8660254037844387076, 1.000000000000000000, 0.8660254037844387076, 1.000000000000000000, 0.8660254037844387076, 1.000000000000000000, 0.8660254037844387076, 1.000000000000000000, 0.8660254037844387076, 1.000000000000000000, 0.8660254037844387076, 1.000000000000000000, 0.8660254037844387076, 1.000000000000000000, 0.8660254037844387076, 1.000000000000000000, 0.9423656443075654199, 0.9343185842653825013 ) ) 
 REPRESENTATION_ITEM ( '' )  );
#4134 = CARTESIAN_POINT ( 'NONE',  ( 34.93719828579781250, 2.096102678619138793, -4.721690477507366701 ) ) ;
#4135 = CARTESIAN_POINT ( 'NONE',  ( 1.767766952966372429, 31.76776695296637598, 13.50000000000000355 ) ) ;
#4136 = CARTESIAN_POINT ( 'NONE',  ( 29.17190429162964094, 2.000000000000001776, 2.500000000000000444 ) ) ;
#4137 = CARTESIAN_POINT ( 'NONE',  ( -25.17020516978313083, 51.00208333237728198, -3.596074190997380349 ) ) ;
#4138 = DIRECTION ( 'NONE',  ( 1.000000000000000000, 0.000000000000000000, 0.000000000000000000 ) ) ;
#4139 = CARTESIAN_POINT ( 'NONE',  ( 2.887392608830349428, 4.041451884327400101, -2.289061810243902218E-14 ) ) ;
#4140 = ORIENTED_EDGE ( 'NONE', *, *, #5357, .T. ) ;
#4141 = CARTESIAN_POINT ( 'NONE',  ( 5.200000000000002842, 0.000000000000000000, 0.000000000000000000 ) ) ;
#4142 = CARTESIAN_POINT ( 'NONE',  ( 4.800000000000000711, 0.000000000000000000, 1.649999999999999911 ) ) ;
#4143 = CARTESIAN_POINT ( 'NONE',  ( -25.17020516978313083, 51.87708333237728198, -3.596074190997380349 ) ) ;
#4144 = AXIS2_PLACEMENT_3D ( 'NONE', #7104, #205, #7885 ) ;
#4145 = CARTESIAN_POINT ( 'NONE',  ( -24.35964822603314417, 54.61874999904395622, -5.000000000000103029 ) ) ;
#4146 = CARTESIAN_POINT ( 'NONE',  ( 22.63806431670481700, 19.48506897666907989, 12.00579112326951758 ) ) ;
#4147 = CARTESIAN_POINT ( 'NONE',  ( -24.98076211353313170, 50.78333333333319644, -3.267949192431250705 ) ) ;
#4148 = ORIENTED_EDGE ( 'NONE', *, *, #7636, .F. ) ;
#4149 = DIRECTION ( 'NONE',  ( 1.000000000000000000, -8.673617379884033500E-16, 0.000000000000000000 ) ) ;
#4150 = ORIENTED_EDGE ( 'NONE', *, *, #6607, .T. ) ;
#4151 = AXIS2_PLACEMENT_3D ( 'NONE', #7611, #1778, #2724 ) ;
#4152 = EDGE_LOOP ( 'NONE', ( #1186, #8455, #6538, #7128, #4716 ) ) ;
#4153 = CARTESIAN_POINT ( 'NONE',  ( 2.000000000000000000, 0.000000000000000000, 0.000000000000000000 ) ) ;
#4154 = ORIENTED_EDGE ( 'NONE', *, *, #6598, .T. ) ;
#4155 = CARTESIAN_POINT ( 'NONE',  ( 2.887392608830845031, -2.020725942164465661, -3.499999999999999556 ) ) ;
#4156 = CARTESIAN_POINT ( 'NONE',  ( 0.000000000000000000, 0.000000000000000000, 0.000000000000000000 ) ) ;
#4157 = EDGE_LOOP ( 'NONE', ( #7751, #5730, #9531 ) ) ;
#4158 = CARTESIAN_POINT ( 'NONE',  ( 17.79249663040192431, 17.21067465782413919, 12.06642298039558980 ) ) ;
#4159 = SHAPE_REPRESENTATION_RELATIONSHIP ( 'NONE' , 'NONE' ,  #716, #7322 ) ;
#4160 = LINE ( 'NONE', #7556, #8073 ) ;
#4161 = AXIS2_PLACEMENT_3D ( 'NONE', #5553, #8933, #4725 ) ;
#4162 = DIRECTION ( 'NONE',  ( -0.000000000000000000, 0.000000000000000000, 1.000000000000000000 ) ) ;
#4163 = EDGE_CURVE ( 'NONE', #702, #1566, #4001, .T. ) ;
#4164 = CARTESIAN_POINT ( 'NONE',  ( 20.29953126043439227, 16.57463755921569515, 12.94889058896590583 ) ) ;
#4165 = CARTESIAN_POINT ( 'NONE',  ( 29.17190429162964094, 7.000000000000002665, 2.500000000000000000 ) ) ;
#4166 = ADVANCED_FACE ( 'NONE', ( #9294 ), #852, .F. ) ;
#4167 = CARTESIAN_POINT ( 'NONE',  ( -23.98076211353314235, 54.25416666475469896, -3.845299461620867554 ) ) ;
#4168 = AXIS2_PLACEMENT_3D ( 'NONE', #1616, #1731, #942 ) ;
#4169 = CONICAL_SURFACE ( 'NONE', #1155, 3.499999999999999556, 1.047197551196603849 ) ;
#4170 = DIRECTION ( 'NONE',  ( -0.000000000000000000, 1.000000000000000000, -0.000000000000000000 ) ) ;
#4171 = ORIENTED_EDGE ( 'NONE', *, *, #2268, .T. ) ;
#4172 = CARTESIAN_POINT ( 'NONE',  ( -26.51666049839534622, 50.31876073720500386, -7.000000000000073719 ) ) ;
#4173 = ORIENTED_EDGE ( 'NONE', *, *, #3630, .T. ) ;
#4174 = VECTOR ( 'NONE', #2913, 1000.000000000000000 ) ;
#4175 = CARTESIAN_POINT ( 'NONE',  ( 3.500000000000005329, 30.00000000000000000, 14.59375000000000178 ) ) ;
#4176 = VECTOR ( 'NONE', #10415, 1000.000000000000000 ) ;
#4177 = CIRCLE ( 'NONE', #9855, 0.5000000000000013323 ) ;
#4178 = ORIENTED_EDGE ( 'NONE', *, *, #6072, .F. ) ;
#4179 = CARTESIAN_POINT ( 'NONE',  ( 19.71976556488538534, 21.01616815698335827, 13.00425721518307753 ) ) ;
#4180 = EDGE_CURVE ( 'NONE', #609, #1386, #5437, .T. ) ;
#4181 = AXIS2_PLACEMENT_3D ( 'NONE', #6239, #2756, #10527 ) ;
#4182 = CARTESIAN_POINT ( 'NONE',  ( 22.86591953417209666, 18.42728137938113875, 11.95042449705224819 ) ) ;
#4183 = DIRECTION ( 'NONE',  ( -0.000000000000000000, -0.000000000000000000, -1.000000000000000000 ) ) ;
#4185 = CARTESIAN_POINT ( 'NONE',  ( 4.750000000000000888, 0.000000000000000000, 0.000000000000000000 ) ) ;
#4184 = AXIS2_PLACEMENT_3D ( 'NONE', #1253, #9803, #5423 ) ;
#4186 = CARTESIAN_POINT ( 'NONE',  ( 1.767766952966372429, 31.76776695296637598, 13.50000000000000355 ) ) ;
#4187 = DIRECTION ( 'NONE',  ( -0.7055570967602625698, 0.7055570967602455834, 0.06616922564518108729 ) ) ;
#4188 = CARTESIAN_POINT ( 'NONE',  ( -25.98076211353324894, 16.50000000000026290, -2.850000000000009859 ) ) ;
#4189 = CARTESIAN_POINT ( 'NONE',  ( 3.199999999999999734, -3.031088913245550298, -1.749999999999972911 ) ) ;
#4190 = EDGE_CURVE ( 'NONE', #6778, #10326, #4737, .T. ) ;
#4191 = EDGE_LOOP ( 'NONE', ( #1332, #4334, #10993, #1659 ) ) ;
#4192 = ORIENTED_EDGE ( 'NONE', *, *, #4794, .T. ) ;
#4193 = CARTESIAN_POINT ( 'NONE',  ( -25.98076211353324894, 14.99999999999984190, -2.500000000000000000 ) ) ;
#4194 = AXIS2_PLACEMENT_3D ( 'NONE', #3741, #6187, #8694 ) ;
#4195 = CARTESIAN_POINT ( 'NONE',  ( -26.51666049839535688, 54.51876073720499249, -7.000000000000071942 ) ) ;
#4196 = CARTESIAN_POINT ( 'NONE',  ( 19.77604874367146692, 21.01153129092389094, 12.00579112326941988 ) ) ;
#4197 = LINE ( 'NONE', #10977, #274 ) ;
#4198 = CARTESIAN_POINT ( 'NONE',  ( 4.000000000000000888, 1.539600717838996990, -3.300726591567079815 ) ) ;
#4199 = CARTESIAN_POINT ( 'NONE',  ( -27.60187600103308014, 52.92708333237728624, -4.064049460664955760 ) ) ;
#4200 = EDGE_CURVE ( 'NONE', #10068, #783, #5200, .T. ) ;
#4201 = FACE_OUTER_BOUND ( 'NONE', #7113, .T. ) ;
#4202 = DIRECTION ( 'NONE',  ( -1.000000000000000000, 0.000000000000000000, 0.000000000000000000 ) ) ;
#4203 = CARTESIAN_POINT ( 'NONE',  ( 4.197310751797292738, 0.8178363989516252985, -3.502498386812444409 ) ) ;
#4204 = ORIENTED_EDGE ( 'NONE', *, *, #10641, .T. ) ;
#4205 = PLANE ( 'NONE',  #8059 ) ;
#4206 = AXIS2_PLACEMENT_3D ( 'NONE', #6591, #10054, #9156 ) ;
#4207 = DIRECTION ( 'NONE',  ( -1.000000000000000000, -6.098637220230963674E-17, 0.000000000000000000 ) ) ;
#4208 =( BOUNDED_SURFACE ( )  B_SPLINE_SURFACE ( 1, 2, ( 
 ( #8277, #4844, #4063, #8172, #8218, #2289, #6553, #4000, #3170, #4113, #662, #7280, #548, #3066, #5626, #1347, #8121, #7445, #9105, #3020, #9842, #7332, #1558, #3947, #10780, #1451, #9951, #6441, #10836, #503, #7389, #2335, #1501, #604, #5728, #3222, #6395, #4746, #4903, #2234, #3899, #9787, #2177, #6600, #10628, #4796, #10000, #5572, #2387, #10675, #5778, #8952, #9011, #9162, #1403, #10720, #4962, #3119, #6496, #9898, #8332, #5678, #9056, #711, #9442, #1788, #5890, #10285, #9336, #4344, #3278, #4167, #10061, #5177, #6724, #10174, #1614, #7560, #3509, #9276, #10946, #6899, #5126, #5012, #6054, #4286, #10117, #6661, #941, #8505, #2679, #885, #827, #8388, #2451, #3338, #2563, #4231, #2504, #7676, #1838, #764, #5838, #7501, #1669 ),
 ( #52, #5068, #8448, #9221, #3455, #8558, #5946, #7620, #2626, #10887, #5231, #6835, #10228, #6004, #1730, #9390, #7731, #111, #3678, #996, #3394, #6776, #8617, #273, #2120, #1161, #10391, #10336, #8675, #4565, #5507, #8775, #2899, #2790, #7951, #9500, #2848, #7161, #2059, #6105, #9557, #8890, #2731, #1957, #5391, #6219, #10454, #1105, #5338, #3564, #4461, #9604, #4509, #3613, #329, #9721, #1900, #5286, #4405, #1050, #6946, #2004, #8006, #7792, #3780, #8724, #3724, #1225, #168, #7842, #7062, #5449, #6166, #7112, #10508, #214, #7001, #7895, #6269, #3670, #9664, #8838, #4621, #378, #10558, #2954, #6328, #4730, #8264, #2321, #648, #9937, #4673, #5714, #3206, #3833, #9092, #1486, #8997, #2371, #4048, #9045, #6539, #4833, #8108 ) ),
 .UNSPECIFIED., .F., .F., .F. ) 
 B_SPLINE_SURFACE_WITH_KNOTS ( ( 2, 2 ),
 ( 3, 2, 2, 2, 2, 2, 2, 2, 2, 2, 2, 2, 2, 2, 2, 2, 2, 2, 2, 2, 2, 2, 2, 2, 2, 2, 2, 2, 2, 2, 2, 2, 2, 2, 2, 2, 2, 2, 2, 2, 2, 2, 2, 2, 2, 2, 2, 2, 2, 2, 2, 2, 3 ),
 ( 0.000000000000000000, 1.000000000000000000 ),
 ( 0.000000000000000000, 0.01851851851851851749, 0.03703703703703703498, 0.05555555555555555247, 0.07407407407407406996, 0.09259259259259258745, 0.1111111111111111049, 0.1296296296296296224, 0.1481481481481481399, 0.1666666666666666574, 0.1851851851851851749, 0.2037037037037036924, 0.2222222222222222099, 0.2407407407407407274, 0.2592592592592592449, 0.2777777777777777901, 0.2962962962962962798, 0.3148148148148148251, 0.3333333333333333148, 0.3518518518518518601, 0.3703703703703703498, 0.3888888888888888951, 0.4074074074074073848, 0.4259259259259259300, 0.4444444444444444198, 0.4629629629629629650, 0.4814814814814814548, 0.5000000000000000000, 0.5185185185185184897, 0.5370370370370370905, 0.5555555555555555802, 0.5740740740740740700, 0.5925925925925925597, 0.6111111111111111605, 0.6296296296296296502, 0.6481481481481481399, 0.6666666666666666297, 0.6851851851851852304, 0.7037037037037037202, 0.7222222222222222099, 0.7407407407407406996, 0.7592592592592593004, 0.7777777777777777901, 0.7962962962962962798, 0.8148148148148147696, 0.8333333333333333703, 0.8518518518518518601, 0.8703703703703703498, 0.8888888888888888395, 0.9074074074074074403, 0.9259259259259259300, 0.9444444444444444198, 0.9524109016187282117 ),
 .UNSPECIFIED. ) 
 GEOMETRIC_REPRESENTATION_ITEM ( )  RATIONAL_B_SPLINE_SURFACE ( (
 ( 1.000000000000000000, 0.8660254037844387076, 1.000000000000000000, 0.8660254037844387076, 1.000000000000000000, 0.8660254037844387076, 1.000000000000000000, 0.8660254037844387076, 1.000000000000000000, 0.8660254037844387076, 1.000000000000000000, 0.8660254037844387076, 1.000000000000000000, 0.8660254037844387076, 1.000000000000000000, 0.8660254037844387076, 1.000000000000000000, 0.8660254037844387076, 1.000000000000000000, 0.8660254037844387076, 1.000000000000000000, 0.8660254037844387076, 1.000000000000000000, 0.8660254037844387076, 1.000000000000000000, 0.8660254037844387076, 1.000000000000000000, 0.8660254037844387076, 1.000000000000000000, 0.8660254037844387076, 1.000000000000000000, 0.8660254037844387076, 1.000000000000000000, 0.8660254037844387076, 1.000000000000000000, 0.8660254037844387076, 1.000000000000000000, 0.8660254037844387076, 1.000000000000000000, 0.8660254037844387076, 1.000000000000000000, 0.8660254037844387076, 1.000000000000000000, 0.8660254037844387076, 1.000000000000000000, 0.8660254037844387076, 1.000000000000000000, 0.8660254037844387076, 1.000000000000000000, 0.8660254037844387076, 1.000000000000000000, 0.8660254037844387076, 1.000000000000000000, 0.8660254037844387076, 1.000000000000000000, 0.8660254037844387076, 1.000000000000000000, 0.8660254037844387076, 1.000000000000000000, 0.8660254037844387076, 1.000000000000000000, 0.8660254037844387076, 1.000000000000000000, 0.8660254037844387076, 1.000000000000000000, 0.8660254037844387076, 1.000000000000000000, 0.8660254037844387076, 1.000000000000000000, 0.8660254037844387076, 1.000000000000000000, 0.8660254037844387076, 1.000000000000000000, 0.8660254037844387076, 1.000000000000000000, 0.8660254037844387076, 1.000000000000000000, 0.8660254037844387076, 1.000000000000000000, 0.8660254037844387076, 1.000000000000000000, 0.8660254037844387076, 1.000000000000000000, 0.8660254037844387076, 1.000000000000000000, 0.8660254037844387076, 1.000000000000000000, 0.8660254037844387076, 1.000000000000000000, 0.8660254037844387076, 1.000000000000000000, 0.8660254037844387076, 1.000000000000000000, 0.8660254037844387076, 1.000000000000000000, 0.8660254037844387076, 1.000000000000000000, 0.8660254037844387076, 1.000000000000000000, 0.8660254037844387076, 1.000000000000000000, 0.8660254037844387076, 1.000000000000000000, 0.9423656443075654199, 0.9343185842653825013),
 ( 1.000000000000000000, 0.8660254037844387076, 1.000000000000000000, 0.8660254037844387076, 1.000000000000000000, 0.8660254037844387076, 1.000000000000000000, 0.8660254037844387076, 1.000000000000000000, 0.8660254037844387076, 1.000000000000000000, 0.8660254037844387076, 1.000000000000000000, 0.8660254037844387076, 1.000000000000000000, 0.8660254037844387076, 1.000000000000000000, 0.8660254037844387076, 1.000000000000000000, 0.8660254037844387076, 1.000000000000000000, 0.8660254037844387076, 1.000000000000000000, 0.8660254037844387076, 1.000000000000000000, 0.8660254037844387076, 1.000000000000000000, 0.8660254037844387076, 1.000000000000000000, 0.8660254037844387076, 1.000000000000000000, 0.8660254037844387076, 1.000000000000000000, 0.8660254037844387076, 1.000000000000000000, 0.8660254037844387076, 1.000000000000000000, 0.8660254037844387076, 1.000000000000000000, 0.8660254037844387076, 1.000000000000000000, 0.8660254037844387076, 1.000000000000000000, 0.8660254037844387076, 1.000000000000000000, 0.8660254037844387076, 1.000000000000000000, 0.8660254037844387076, 1.000000000000000000, 0.8660254037844387076, 1.000000000000000000, 0.8660254037844387076, 1.000000000000000000, 0.8660254037844387076, 1.000000000000000000, 0.8660254037844387076, 1.000000000000000000, 0.8660254037844387076, 1.000000000000000000, 0.8660254037844387076, 1.000000000000000000, 0.8660254037844387076, 1.000000000000000000, 0.8660254037844387076, 1.000000000000000000, 0.8660254037844387076, 1.000000000000000000, 0.8660254037844387076, 1.000000000000000000, 0.8660254037844387076, 1.000000000000000000, 0.8660254037844387076, 1.000000000000000000, 0.8660254037844387076, 1.000000000000000000, 0.8660254037844387076, 1.000000000000000000, 0.8660254037844387076, 1.000000000000000000, 0.8660254037844387076, 1.000000000000000000, 0.8660254037844387076, 1.000000000000000000, 0.8660254037844387076, 1.000000000000000000, 0.8660254037844387076, 1.000000000000000000, 0.8660254037844387076, 1.000000000000000000, 0.8660254037844387076, 1.000000000000000000, 0.8660254037844387076, 1.000000000000000000, 0.8660254037844387076, 1.000000000000000000, 0.8660254037844387076, 1.000000000000000000, 0.8660254037844387076, 1.000000000000000000, 0.8660254037844387076, 1.000000000000000000, 0.8660254037844387076, 1.000000000000000000, 0.9423656443075654199, 0.9343185842653825013) ) ) 
 REPRESENTATION_ITEM ( '' )  SURFACE ( )  );
#4209 = CARTESIAN_POINT ( 'NONE',  ( -27.60187600103308725, 55.78541666571062052, -5.935950539335252074 ) ) ;
#4210 = CARTESIAN_POINT ( 'NONE',  ( 25.98076211353324183, 54.99999999999984368, 2.500000000000000000 ) ) ;
#4211 = LINE ( 'NONE', #869, #4840 ) ;
#4212 = AXIS2_PLACEMENT_3D ( 'NONE', #9861, #622, #5853 ) ;
#4213 = CIRCLE ( 'NONE', #2096, 1.999999999999971356 ) ;
#4214 = CARTESIAN_POINT ( 'NONE',  ( -27.98076211353308551, 51.94999999999986784, -5.000000000000103029 ) ) ;
#4215 = ORIENTED_EDGE ( 'NONE', *, *, #8444, .F. ) ;
#4216 = ORIENTED_EDGE ( 'NONE', *, *, #7569, .F. ) ;
#4217 = ORIENTED_EDGE ( 'NONE', *, *, #10142, .T. ) ;
#4218 = CARTESIAN_POINT ( 'NONE',  ( -30.98076211353324894, 14.99999999999984190, 2.500000000000000000 ) ) ;
#4219 = ORIENTED_EDGE ( 'NONE', *, *, #839, .T. ) ;
#4220 = FACE_OUTER_BOUND ( 'NONE', #8046, .T. ) ;
#4221 = DIRECTION ( 'NONE',  ( -1.000000000000000000, 0.000000000000000000, -6.982962677686266711E-15 ) ) ;
#4222 = ORIENTED_EDGE ( 'NONE', *, *, #9998, .F. ) ;
#4223 = CARTESIAN_POINT ( 'NONE',  ( 20.05583492806123758, 17.75628287944761396, 11.00732503135576401 ) ) ;
#4224 = DIRECTION ( 'NONE',  ( 0.000000000000000000, 0.000000000000000000, -1.000000000000000000 ) ) ;
#4225 = EDGE_CURVE ( 'NONE', #6073, #6168, #10927, .T. ) ;
#4226 = CARTESIAN_POINT ( 'NONE',  ( -4.000000000000000000, 0.7924765000094600165, -0.05906175389889745803 ) ) ;
#4227 =( REPRESENTATION_RELATIONSHIP ('NONE','NONE', #7540, #1223 ) REPRESENTATION_RELATIONSHIP_WITH_TRANSFORMATION ( #1273 )SHAPE_REPRESENTATION_RELATIONSHIP( ) );
#4228 = CARTESIAN_POINT ( 'NONE',  ( 2.886521338340684917, 0.000000000000000000, 0.000000000000000000 ) ) ;
#4229 = CARTESIAN_POINT ( 'NONE',  ( 20.23629815768686768, 16.66554095800588797, 10.95195840513859231 ) ) ;
#4230 = DIRECTION ( 'NONE',  ( 0.000000000000000000, 0.000000000000000000, 1.000000000000000000 ) ) ;
#4231 = CARTESIAN_POINT ( 'NONE',  ( -23.98076211353314235, 55.77083333142137178, -6.154700538379337615 ) ) ;
#4232 = VECTOR ( 'NONE', #10572, 1000.000000000000000 ) ;
#4233 = STYLED_ITEM ( 'NONE', ( #176 ), #2840 ) ;
#4234 = CARTESIAN_POINT ( 'NONE',  ( -23.98076211353314235, 53.64166666666653072, -3.845299461620867554 ) ) ;
#4235 = ORIENTED_EDGE ( 'NONE', *, *, #5215, .T. ) ;
#4236 = CARTESIAN_POINT ( 'NONE',  ( -25.00795256721317372, 58.26617124284993565, -3.251596195468438033 ) ) ;
#4237 = ORIENTED_EDGE ( 'NONE', *, *, #8319, .F. ) ;
#4238 = VECTOR ( 'NONE', #7135, 1000.000000000000000 ) ;
#4239 = CARTESIAN_POINT ( 'NONE',  ( 1.515916693951011140, 26.52740819067395250, 13.36156658473306535 ) ) ;
#4240 = ORIENTED_EDGE ( 'NONE', *, *, #253, .T. ) ;
#4241 = EDGE_CURVE ( 'NONE', #8894, #3195, #9357, .T. ) ;
#4242 = CARTESIAN_POINT ( 'NONE',  ( 20.39832466968983837, 22.29813831026750393, 13.00425721518307753 ) ) ;
#4243 = EDGE_CURVE ( 'NONE', #491, #6512, #8438, .T. ) ;
#4244 = CARTESIAN_POINT ( 'NONE',  ( -25.98076211353310683, 53.52499999999986358, -3.000000000000132339 ) ) ;
#4245 = FACE_OUTER_BOUND ( 'NONE', #5088, .T. ) ;
#4246 = DIRECTION ( 'NONE',  ( 1.000000000000000000, -0.000000000000000000, 1.156482317317871478E-16 ) ) ;
#4247 = CARTESIAN_POINT ( 'NONE',  ( -1.767766952966375094, 31.76776695296636888, 13.81250000000000355 ) ) ;
#4248 = DIRECTION ( 'NONE',  ( 0.000000000000000000, 0.000000000000000000, -1.000000000000000000 ) ) ;
#4249 = CARTESIAN_POINT ( 'NONE',  ( 34.99999999999987210, -17.99999999999996803, 7.500000000000038192 ) ) ;
#4250 = CARTESIAN_POINT ( 'NONE',  ( 0.000000000000000000, 0.000000000000000000, 0.000000000000000000 ) ) ;
#4251 = EDGE_LOOP ( 'NONE', ( #705, #2208, #4276 ) ) ;
#4252 = ADVANCED_FACE ( 'NONE', ( #1636 ), #785, .T. ) ;
#4253 = ORIENTED_EDGE ( 'NONE', *, *, #5298, .F. ) ;
#4254 = ADVANCED_FACE ( 'NONE', ( #10136 ), #5089, .T. ) ;
#4255 = DIRECTION ( 'NONE',  ( 0.000000000000000000, 1.000000000000000000, 0.000000000000000000 ) ) ;
#4256 = CARTESIAN_POINT ( 'NONE',  ( -25.98076211353311393, 54.48749999808803324, -7.000000000000072831 ) ) ;
#4257 = CARTESIAN_POINT ( 'NONE',  ( 20.47715220320264962, 17.98190999816754498, 12.00579112326941988 ) ) ;
#4258 = CARTESIAN_POINT ( 'NONE',  ( 1.767766952966372429, 31.76776695296637598, 16.00000000000000355 ) ) ;
#4259 = DIRECTION ( 'NONE',  ( 1.000000000000000000, 0.000000000000000000, 0.000000000000000000 ) ) ;
#4260 = CARTESIAN_POINT ( 'NONE',  ( -24.35964822603314417, 53.21874999904395764, -5.000000000000103029 ) ) ;
#4261 = CARTESIAN_POINT ( 'NONE',  ( -24.35964822603314417, 49.89374999904394770, -5.000000000000103029 ) ) ;
#4262 = DIRECTION ( 'NONE',  ( -1.000000000000000000, 0.000000000000000000, 0.000000000000000000 ) ) ;
#4263 = CARTESIAN_POINT ( 'NONE',  ( 2.000000000000008882, 3.464101615137749945, 0.000000000000000000 ) ) ;
#4264 = ORIENTED_EDGE ( 'NONE', *, *, #10502, .T. ) ;
#4265 = LINE ( 'NONE', #7651, #1856 ) ;
#4266 = CARTESIAN_POINT ( 'NONE',  ( 29.49999999999999645, -3.999999999999986233, -4.999999999999991118 ) ) ;
#4267 = CARTESIAN_POINT ( 'NONE',  ( -25.98076211353310683, 52.16874999904395338, -6.871901078670399343 ) ) ;
#4268 = CARTESIAN_POINT ( 'NONE',  ( -23.98076211353314235, 50.84166666666652645, -3.845299461620867554 ) ) ;
#4269 = B_SPLINE_CURVE_WITH_KNOTS ( 'NONE', 3,
 ( #9875, #8930, #9820, #9767, #417, #5603, #2265, #579 ),
 .UNSPECIFIED., .F., .F.,
 ( 4, 2, 2, 4 ),
 ( 2.465131517390770070E-07, 0.001183067374689869946, 0.001774477805458935659, 0.002365888236228001588 ),
 .UNSPECIFIED. ) ;
#4270 = CARTESIAN_POINT ( 'NONE',  ( 25.58039891549807976, 2.000000000000002665, 17.50099999999999767 ) ) ;
#4271 = CARTESIAN_POINT ( 'NONE',  ( -25.98076211353311393, 51.77499999999986358, -7.309401076758571314 ) ) ;
#4272 = VERTEX_POINT ( 'NONE', #9465 ) ;
#4273 =( BOUNDED_CURVE ( )  B_SPLINE_CURVE ( 2, ( #3813, #7254, #6372, #9760, #2152, #1311, #8707, #1086, #2880 ),
 .UNSPECIFIED., .F., .F. ) 
 B_SPLINE_CURVE_WITH_KNOTS ( ( 3, 2, 2, 2, 3 ),
 ( 0.5277777777777777901, 0.5370370370370370905, 0.5555555555555555802, 0.5740740740740740700, 0.5833333333333333703 ),
 .UNSPECIFIED. ) 
 CURVE ( )  GEOMETRIC_REPRESENTATION_ITEM ( )  RATIONAL_B_SPLINE_CURVE ( ( 0.9330127018922194093, 0.9330127018922194093, 1.000000000000000000, 0.8660254037844387076, 1.000000000000000000, 0.8660254037844387076, 1.000000000000000000, 0.9330127018922189652, 0.9330127018922194093 ) ) 
 REPRESENTATION_ITEM ( '' )  );
#4274 = VERTEX_POINT ( 'NONE', #294 ) ;
#4275 = CARTESIAN_POINT ( 'NONE',  ( -25.98076211353324894, 16.50000000000026290, -2.850000000000008082 ) ) ;
#4276 = ORIENTED_EDGE ( 'NONE', *, *, #7098, .F. ) ;
#4277 = CARTESIAN_POINT ( 'NONE',  ( 0.000000000000000000, 0.000000000000000000, -5.000000000000000000 ) ) ;
#4278 = FILL_AREA_STYLE ('',( #3328 ) ) ;
#4279 = ORIENTED_EDGE ( 'NONE', *, *, #4527, .F. ) ;
#4280 = CARTESIAN_POINT ( 'NONE',  ( 22.63806431670481700, 19.48506897666907989, 12.00579112326951758 ) ) ;
#4281 = DIRECTION ( 'NONE',  ( 0.000000000000000000, -1.000000000000000000, 0.000000000000000000 ) ) ;
#4282 = FACE_OUTER_BOUND ( 'NONE', #9828, .T. ) ;
#4283 = CARTESIAN_POINT ( 'NONE',  ( 21.82671760412675610, 17.70440453107251244, 11.95042449705224819 ) ) ;
#4284 = CARTESIAN_POINT ( 'NONE',  ( -3.679171394226034675, -2.494631558665844739, -0.3503314178412558211 ) ) ;
#4285 = DIRECTION ( 'NONE',  ( -1.000000000000000000, 0.000000000000000000, 0.000000000000000000 ) ) ;
#4286 = CARTESIAN_POINT ( 'NONE',  ( -23.98076211353314235, 55.07083333142136894, -6.154700538379337615 ) ) ;
#4287 = AXIS2_PLACEMENT_3D ( 'NONE', #349, #7187, #6241 ) ;
#4288 = CARTESIAN_POINT ( 'NONE',  ( -25.98076211353324894, 16.50000000000026290, -5.000000000000000000 ) ) ;
#4289 = ORIENTED_EDGE ( 'NONE', *, *, #9663, .T. ) ;
#4290 = AXIS2_PLACEMENT_3D ( 'NONE', #3456, #9443, #3511 ) ;
#4291 = LINE ( 'NONE', #7679, #5473 ) ;
#4292 = ORIENTED_EDGE ( 'NONE', *, *, #7162, .F. ) ;
#4293 = CARTESIAN_POINT ( 'NONE',  ( 2.521662442312487151, 27.57191497400665270, 14.68969158473306535 ) ) ;
#4294 = ORIENTED_EDGE ( 'NONE', *, *, #1393, .T. ) ;
#4295 = CARTESIAN_POINT ( 'NONE',  ( 23.58716357997163016, 18.92604383881832675, 12.94889058896590583 ) ) ;
#4296 = DIRECTION ( 'NONE',  ( 0.000000000000000000, 0.000000000000000000, 1.000000000000000000 ) ) ;
#4297 = CARTESIAN_POINT ( 'NONE',  ( -25.47290043343602051, 58.87139657625925082, -6.938381116177147589 ) ) ;
#4298 = CARTESIAN_POINT ( 'NONE',  ( 17.79249663040192431, 17.21067465782413919, 12.06642298039558980 ) ) ;
#4299 = CARTESIAN_POINT ( 'NONE',  ( -27.60187600103308014, 52.81041666571061199, -5.935950539335252074 ) ) ;
#4300 = CARTESIAN_POINT ( 'NONE',  ( -26.25045812061784289, 0.000000000000000000, -9.500000000000000000 ) ) ;
#4301 = DIRECTION ( 'NONE',  ( -0.7055570967602625698, 0.7055570967602456944, 0.06616922564518108729 ) ) ;
#4302 = DIRECTION ( 'NONE',  ( 0.000000000000000000, 0.000000000000000000, -1.000000000000000000 ) ) ;
#4303 = CARTESIAN_POINT ( 'NONE',  ( -26.94773701350929329, 58.26330508548400644, -6.750767313052078222 ) ) ;
#4304 = B_SPLINE_CURVE_WITH_KNOTS ( 'NONE', 3,
 ( #9164, #9107, #714, #2337, #9058, #665 ),
 .UNSPECIFIED., .F., .F.,
 ( 4, 2, 4 ),
 ( 0.008988604078116352661, 0.01001254935948927942, 0.01103649464086220618 ),
 .UNSPECIFIED. ) ;
#4305 = VERTEX_POINT ( 'NONE', #7970 ) ;
#4306 = ORIENTED_EDGE ( 'NONE', *, *, #2031, .F. ) ;
#4307 = CARTESIAN_POINT ( 'NONE',  ( -26.51666049839534622, 51.80626073911682283, -7.000000000000073719 ) ) ;
#4308 = DIRECTION ( 'NONE',  ( 1.000000000000000000, -0.000000000000000000, 1.156482317317871478E-16 ) ) ;
#4309 = CARTESIAN_POINT ( 'NONE',  ( 34.92408131826246631, 2.305272916965852570, -4.166859826334558647 ) ) ;
#4310 = VECTOR ( 'NONE', #10750, 1000.000000000000000 ) ;
#4311 = CARTESIAN_POINT ( 'NONE',  ( -23.98076211353314235, 55.77083333142137178, -6.154700538379337615 ) ) ;
#4312 = EDGE_CURVE ( 'NONE', #1351, #6840, #1857, .T. ) ;
#4313 = CARTESIAN_POINT ( 'NONE',  ( 4.235886605889389145, 2.417314728048528760, -3.751161874094018245 ) ) ;
#4314 = CARTESIAN_POINT ( 'NONE',  ( -24.35964822603314772, 55.26041666571062194, -4.064049460664953983 ) ) ;
#4315 = ADVANCED_FACE ( 'NONE', ( #2753 ), #10413, .T. ) ;
#4316 = FACE_OUTER_BOUND ( 'NONE', #10872, .T. ) ;
#4317 = CARTESIAN_POINT ( 'NONE',  ( 5.621179405865834866, 34.96511249490581008, 0.000000000000000000 ) ) ;
#4318 = CARTESIAN_POINT ( 'NONE',  ( 2.345747346278113987, -3.264484291692503870, -0.01223254789874484924 ) ) ;
#4319 = ORIENTED_EDGE ( 'NONE', *, *, #9220, .F. ) ;
#4320 = CARTESIAN_POINT ( 'NONE',  ( -25.71106610644865498, 13.49999999999941913, -9.500000000000000000 ) ) ;
#4321 = DIRECTION ( 'NONE',  ( 0.000000000000000000, 0.000000000000000000, 1.000000000000000000 ) ) ;
#4322 = CARTESIAN_POINT ( 'NONE',  ( -25.98076211353310683, 55.31874999904394485, -3.128098921329806714 ) ) ;
#4323 = CARTESIAN_POINT ( 'NONE',  ( -25.44486372867087454, 51.04373926088290858, -7.000000000000073719 ) ) ;
#4324 = EDGE_CURVE ( 'NONE', #7995, #5562, #6236, .T. ) ;
#4325 =( BOUNDED_CURVE ( )  B_SPLINE_CURVE ( 2, ( #8924, #1312, #8147, #469, #2257, #8039, #3871, #3041, #6415 ),
 .UNSPECIFIED., .F., .F. ) 
 B_SPLINE_CURVE_WITH_KNOTS ( ( 3, 2, 2, 2, 3 ),
 ( 0.3055555555555555802, 0.3148148148148148251, 0.3333333333333333148, 0.3518518518518518601, 0.3611111111111111049 ),
 .UNSPECIFIED. ) 
 CURVE ( )  GEOMETRIC_REPRESENTATION_ITEM ( )  RATIONAL_B_SPLINE_CURVE ( ( 0.9330127018922194093, 0.9330127018922195203, 1.000000000000000000, 0.8660254037844387076, 1.000000000000000000, 0.8660254037844387076, 1.000000000000000000, 0.9330127018922194093, 0.9330127018922194093 ) ) 
 REPRESENTATION_ITEM ( '' )  );
#4326 = FACE_OUTER_BOUND ( 'NONE', #6387, .T. ) ;
#4327 = CARTESIAN_POINT ( 'NONE',  ( -26.98076211353309972, 51.13333333333319786, -6.732050807568954909 ) ) ;
#4328 = ORIENTED_EDGE ( 'NONE', *, *, #7475, .F. ) ;
#4329 = ORIENTED_EDGE ( 'NONE', *, *, #8859, .T. ) ;
#4330 = CARTESIAN_POINT ( 'NONE',  ( 0.1397399040437465878, 1.362955318038519659, -3.499999999999999556 ) ) ;
#4331 = ADVANCED_FACE ( 'NONE', ( #185 ), #3584, .F. ) ;
#4332 = CARTESIAN_POINT ( 'NONE',  ( 3.061857526609890190, -1.355358988605575021, -3.499999999999999556 ) ) ;
#4333 = SHAPE_DEFINITION_REPRESENTATION ( #2103, #3016 ) ;
#4334 = ORIENTED_EDGE ( 'NONE', *, *, #6882, .F. ) ;
#4335 = CARTESIAN_POINT ( 'NONE',  ( 22.44007493706583745, 19.34731747087121434, 12.00579112326928133 ) ) ;
#4336 = DIRECTION ( 'NONE',  ( -0.000000000000000000, 1.000000000000000000, -0.000000000000000000 ) ) ;
#4337 = CARTESIAN_POINT ( 'NONE',  ( -26.51666049839535333, 52.00623925897107114, -3.000000000000132339 ) ) ;
#4338 = DIRECTION ( 'NONE',  ( -1.000000000000000000, -0.000000000000000000, -0.000000000000000000 ) ) ;
#4339 = CARTESIAN_POINT ( 'NONE',  ( 20.77365933115271446, 23.55783661745384094, 11.95042449705224819 ) ) ;
#4340 =( REPRESENTATION_RELATIONSHIP ('NONE','NONE', #7540, #7975 ) REPRESENTATION_RELATIONSHIP_WITH_TRANSFORMATION ( #2891 )SHAPE_REPRESENTATION_RELATIONSHIP( ) );
#4341 = AXIS2_PLACEMENT_3D ( 'NONE', #3147, #6529, #9928 ) ;
#4342 = EDGE_CURVE ( 'NONE', #1437, #40, #1016, .T. ) ;
#4343 = DIRECTION ( 'NONE',  ( -1.000000000000000000, 0.000000000000000000, 0.000000000000000000 ) ) ;
#4344 = CARTESIAN_POINT ( 'NONE',  ( -25.98076211353311393, 54.13749999808803182, -2.690598923241634743 ) ) ;
#4345 = CARTESIAN_POINT ( 'NONE',  ( -23.98076211353314235, 53.75833333333319786, -6.154700538379337615 ) ) ;
#4346 = EDGE_LOOP ( 'NONE', ( #8114, #5498, #4049, #8317 ) ) ;
#4347 = CARTESIAN_POINT ( 'NONE',  ( 2.500000000000000000, 2.500728763858895382E-16, -2.041999999999999815 ) ) ;
#4348 = VERTEX_POINT ( 'NONE', #2811 ) ;
#4349 = CARTESIAN_POINT ( 'NONE',  ( 3.500000000000003997, 30.06616922564517580, 13.59594158473306358 ) ) ;
#4350 = VECTOR ( 'NONE', #5539, 1000.000000000000000 ) ;
#4351 = EDGE_LOOP ( 'NONE', ( #3570, #4499 ) ) ;
#4352 = CARTESIAN_POINT ( 'NONE',  ( 23.83741617020655212, 22.59052263540754524, 12.94889058896590583 ) ) ;
#4353 = CIRCLE ( 'NONE', #10555, 2.200000000000001066 ) ;
#4354 = CARTESIAN_POINT ( 'NONE',  ( 2.550604951803072673, 0.000000000000000000, 0.000000000000000000 ) ) ;
#4355 = CARTESIAN_POINT ( 'NONE',  ( 22.82387490247590733, 19.65457484615246386, 12.00579112326941988 ) ) ;
#4356 = CARTESIAN_POINT ( 'NONE',  ( -25.17020516978313083, 50.53541666571062052, -6.403925809002825709 ) ) ;
#4357 = AXIS2_PLACEMENT_3D ( 'NONE', #4210, #2774, #6146 ) ;
#4358 = CLOSED_SHELL ( 'NONE', ( #1590, #4426, #5569, #6023, #7304, #146, #5928, #10211, #9636, #3708, #919, #10734, #6820, #1880, #6359, #10822, #291, #7027, #10353, #8376, #4331, #2333, #227, #1807, #440, #8998, #282 ) ) ;
#4359 = LINE ( 'NONE', #3577, #10970 ) ;
#4360 = CIRCLE ( 'NONE', #10567, 2.649999999999992362 ) ;
#4361 = CARTESIAN_POINT ( 'NONE',  ( -6.921953244962140004E-15, -2.859595677584344298, 2.047034997319538085 ) ) ;
#4362 = PLANE ( 'NONE',  #5984 ) ;
#4363 = ORIENTED_EDGE ( 'NONE', *, *, #2625, .F. ) ;
#4364 = ORIENTED_EDGE ( 'NONE', *, *, #3580, .T. ) ;
#4365 = CARTESIAN_POINT ( 'NONE',  ( 18.62184541094303114, 16.98042197548449295, 12.02177981800743112 ) ) ;
#4366 = AXIS2_PLACEMENT_3D ( 'NONE', #6447, #7340, #2296 ) ;
#4367 = CARTESIAN_POINT ( 'NONE',  ( 29.49999999999999645, -3.999999999999986233, -4.999999999999991118 ) ) ;
#4368 = CARTESIAN_POINT ( 'NONE',  ( 34.74482695545609801, 4.223122737142881000, -2.595677240809972641 ) ) ;
#4369 = AXIS2_PLACEMENT_3D ( 'NONE', #2822, #9581, #6194 ) ;
#4370 = ADVANCED_FACE ( 'NONE', ( #4429 ), #4526, .T. ) ;
#4371 = CARTESIAN_POINT ( 'NONE',  ( -27.98076211353308551, 52.59166666666651935, -6.154700538379338504 ) ) ;
#4372 = DIRECTION ( 'NONE',  ( 0.000000000000000000, 1.000000000000000000, -1.471414886128461471E-15 ) ) ;
#4373 = CARTESIAN_POINT ( 'NONE',  ( -27.60187600103308014, 54.32708333237728482, -4.064049460664955760 ) ) ;
#4374 = DIRECTION ( 'NONE',  ( -1.000000000000000000, -6.098637220230964906E-17, 0.000000000000000000 ) ) ;
#4375 = CARTESIAN_POINT ( 'NONE',  ( 2.290893957444128645E-15, 4.647089433458768681, -3.572167766733382877 ) ) ;
#4376 = CARTESIAN_POINT ( 'NONE',  ( 2.687328764639642653, -3.067272167851299969, -0.05923475698271395140 ) ) ;
#4377 = VERTEX_POINT ( 'NONE', #6967 ) ;
#4378 = CARTESIAN_POINT ( 'NONE',  ( 24.99999259214812142, 30.01924558493218598, -2.500000000000000000 ) ) ;
#4379 = CIRCLE ( 'NONE', #6142, 2.500000000000001332 ) ;
#4380 = CARTESIAN_POINT ( 'NONE',  ( 1.814555661125939467, 31.72097824480680828, 16.99780841526693820 ) ) ;
#4381 = CARTESIAN_POINT ( 'NONE',  ( -2.500000000000004441, 28.96446609406725159, 15.29687500000000178 ) ) ;
#4382 = APPLICATION_CONTEXT ( 'automotive_design' ) ;
#4383 = ADVANCED_FACE ( 'NONE', ( #7082 ), #3688, .T. ) ;
#4384 = CARTESIAN_POINT ( 'NONE',  ( -26.79131905728310059, 55.26041666571061484, -3.596074190997381237 ) ) ;
#4385 = CARTESIAN_POINT ( 'NONE',  ( 4.000000000000000000, -2.309401076758514915, -5.000000000000000000 ) ) ;
#4386 = ADVANCED_FACE ( 'NONE', ( #1973 ), #1919, .F. ) ;
#4387 = AXIS2_PLACEMENT_3D ( 'NONE', #8799, #7083, #3586 ) ;
#4388 = CARTESIAN_POINT ( 'NONE',  ( 5.200000000000002842, 0.000000000000000000, 0.000000000000000000 ) ) ;
#4389 = CARTESIAN_POINT ( 'NONE',  ( 15.87890888817147150, 17.65662501776163040, 12.17661548709639696 ) ) ;
#4390 = ORIENTED_EDGE ( 'NONE', *, *, #7287, .F. ) ;
#4391 = VERTEX_POINT ( 'NONE', #1808 ) ;
#4392 = FACE_OUTER_BOUND ( 'NONE', #730, .T. ) ;
#4393 = EDGE_CURVE ( 'NONE', #10063, #4377, #5308, .T. ) ;
#4394 = CARTESIAN_POINT ( 'NONE',  ( 0.000000000000000000, 0.000000000000000000, 2.500000000000000000 ) ) ;
#4395 = APPLICATION_PROTOCOL_DEFINITION ( 'draft international standard', 'automotive_design', 1998, #1170 ) ;
#4396 = ORIENTED_EDGE ( 'NONE', *, *, #10570, .F. ) ;
#4397 = LINE ( 'NONE', #819, #9672 ) ;
#4398 = CARTESIAN_POINT ( 'NONE',  ( 34.99999999999999289, -3.999999999999993339, -2.850000000000003642 ) ) ;
#4399 = VECTOR ( 'NONE', #182, 1000.000000000000000 ) ;
#4400 = AXIS2_PLACEMENT_3D ( 'NONE', #8494, #3267, #9098 ) ;
#4401 = ADVANCED_FACE ( 'NONE', ( #7129 ), #9576, .T. ) ;
#4402 = EDGE_CURVE ( 'NONE', #3459, #7216, #8814, .T. ) ;
#4403 = CARTESIAN_POINT ( 'NONE',  ( 17.34774915531493278, 16.33073436721105054, 11.04457336562047765 ) ) ;
#4404 = DIRECTION ( 'NONE',  ( 0.000000000000000000, 0.000000000000000000, -1.000000000000000000 ) ) ;
#4405 = CARTESIAN_POINT ( 'NONE',  ( -25.17020516978313083, 53.27708333237728056, -3.596074190997380349 ) ) ;
#4406 = B_SPLINE_CURVE_WITH_KNOTS ( 'NONE', 3,
 ( #4087, #5751, #9815, #688, #9193, #2202, #8982, #3093 ),
 .UNSPECIFIED., .F., .F.,
 ( 4, 2, 2, 4 ),
 ( 2.465131517075058656E-07, 0.001183067374689851080, 0.001774477805458923299, 0.002365888236227995517 ),
 .UNSPECIFIED. ) ;
#4407 = CARTESIAN_POINT ( 'NONE',  ( 25.71106610644839208, 56.49999999999984368, 10.00000000000000178 ) ) ;
#4408 = ORIENTED_EDGE ( 'NONE', *, *, #7649, .T. ) ;
#4409 = DIRECTION ( 'NONE',  ( 1.000000000000000000, 0.000000000000000000, 0.000000000000000000 ) ) ;
#4410 = PRODUCT_DEFINITION_SHAPE ( 'NONE', 'NONE',  #11000 ) ;
#4411 = EDGE_LOOP ( 'NONE', ( #5910, #8111, #8513, #3486 ) ) ;
#4412 = VECTOR ( 'NONE', #2734, 1000.000000000000114 ) ;
#4413 = VECTOR ( 'NONE', #9103, 1000.000000000000000 ) ;
#4414 = CARTESIAN_POINT ( 'NONE',  ( 1.383578242660657098, 33.52740819067396671, 13.83031658473306535 ) ) ;
#4415 = ORIENTED_EDGE ( 'NONE', *, *, #441, .T. ) ;
#4416 = CARTESIAN_POINT ( 'NONE',  ( 19.07396262421655919, 19.44200532275891291, 12.94889058896472811 ) ) ;
#4417 = CARTESIAN_POINT ( 'NONE',  ( 25.98076211353311749, 53.49999999999983658, 7.850000000000012967 ) ) ;
#4418 = CIRCLE ( 'NONE', #5485, 3.499999999999999556 ) ;
#4419 =( GEOMETRIC_REPRESENTATION_CONTEXT ( 3 ) GLOBAL_UNCERTAINTY_ASSIGNED_CONTEXT ( ( #5322 ) ) GLOBAL_UNIT_ASSIGNED_CONTEXT ( ( #3894, #9008, #3679 ) ) REPRESENTATION_CONTEXT ( 'NONE', 'WORKASPACE' ) );
#4420 = CARTESIAN_POINT ( 'NONE',  ( -27.60187600103308014, 52.11041666571061626, -5.935950539335252074 ) ) ;
#4421 = AXIS2_PLACEMENT_3D ( 'NONE', #737, #4138, #7590 ) ;
#4422 = CARTESIAN_POINT ( 'NONE',  ( 1.035533905932737975, 32.50000000000000711, 16.07812500000000355 ) ) ;
#4423 = CARTESIAN_POINT ( 'NONE',  ( 29.49999999999999289, -3.999999999999993339, 7.850000000000016520 ) ) ;
#4424 = DIRECTION ( 'NONE',  ( 6.098637220230961209E-17, -1.000000000000000000, 1.807003620809174139E-16 ) ) ;
#4425 = ORIENTED_EDGE ( 'NONE', *, *, #418, .F. ) ;
#4426 = ADVANCED_FACE ( 'NONE', ( #8875 ), #6857, .T. ) ;
#4427 = ORIENTED_EDGE ( 'NONE', *, *, #10502, .F. ) ;
#4428 = VECTOR ( 'NONE', #2426, 1000.000000000000000 ) ;
#4429 = FACE_OUTER_BOUND ( 'NONE', #203, .T. ) ;
#4430 = FACE_OUTER_BOUND ( 'NONE', #6613, .T. ) ;
#4431 = AXIS2_PLACEMENT_3D ( 'NONE', #4165, #7559, #8135 ) ;
#4432 = CARTESIAN_POINT ( 'NONE',  ( -2.649999999999885780, 30.00000000000000000, 2.500000000000000000 ) ) ;
#4433 = CARTESIAN_POINT ( 'NONE',  ( -25.98076211353311393, 52.47499999999985931, -7.000000000000072831 ) ) ;
#4434 = CARTESIAN_POINT ( 'NONE',  ( 1.287237434362044075, 3.875615274277557809, -3.430618716626812059 ) ) ;
#4435 = CARTESIAN_POINT ( 'NONE',  ( -25.17020516978313083, 55.20208333237728482, -3.596074190997380349 ) ) ;
#4436 = DIRECTION ( 'NONE',  ( 0.000000000000000000, 1.000000000000000000, 0.000000000000000000 ) ) ;
#4437 = DIRECTION ( 'NONE',  ( -6.308085367188384325E-16, -3.847072420872938447E-32, 1.000000000000000000 ) ) ;
#4438 = CARTESIAN_POINT ( 'NONE',  ( 3.355112389629172576, -2.681727112203168950, -0.2256878752776777242 ) ) ;
#4439 = ORIENTED_EDGE ( 'NONE', *, *, #1924, .T. ) ;
#4440 = DIRECTION ( 'NONE',  ( 1.000000000000000000, 0.000000000000000000, 0.000000000000000000 ) ) ;
#4441 = CARTESIAN_POINT ( 'NONE',  ( 1.035533905932743970, 27.49999999999999289, 15.60937500000000711 ) ) ;
#4442 = CARTESIAN_POINT ( 'NONE',  ( -1.035533905932742638, 32.50000000000000000, 14.98437500000000711 ) ) ;
#4443 = UNCERTAINTY_MEASURE_WITH_UNIT (LENGTH_MEASURE( 1.000000000000000082E-05 ), #9003, 'distance_accuracy_value', 'NONE');
#4444 = CARTESIAN_POINT ( 'NONE',  ( -25.17020516978313083, 55.61041666571061626, -6.403925809002825709 ) ) ;
#4445 = CARTESIAN_POINT ( 'NONE',  ( -23.98076211353314235, 55.04166666666652930, -3.845299461620867554 ) ) ;
#4446 = CARTESIAN_POINT ( 'NONE',  ( 34.99999999999999289, 2.000000000000002220, -10.50000000000000355 ) ) ;
#4447 = CARTESIAN_POINT ( 'NONE',  ( -23.98076211353314235, 54.34166666666652645, -3.845299461620867554 ) ) ;
#4448 = PRODUCT_RELATED_PRODUCT_CATEGORY ( 'part', '', ( #9165 ) ) ;
#4449 = EDGE_LOOP ( 'NONE', ( #9379, #8189, #3687, #2119 ) ) ;
#4450 = ORIENTED_EDGE ( 'NONE', *, *, #3599, .F. ) ;
#4451 = CARTESIAN_POINT ( 'NONE',  ( -23.98076211353314235, 50.75416666475469896, -3.845299461620867554 ) ) ;
#4452 = CARTESIAN_POINT ( 'NONE',  ( 3.200000000000000178, -4.041451884327390331, 2.328587628042611615E-14 ) ) ;
#4453 = SHAPE_DEFINITION_REPRESENTATION ( #9629, #1223 ) ;
#4454 = ORIENTED_EDGE ( 'NONE', *, *, #3909, .F. ) ;
#4455 = DIRECTION ( 'NONE',  ( 1.000000000000000000, 6.098637220230963674E-17, 0.000000000000000000 ) ) ;
#4456 = CARTESIAN_POINT ( 'NONE',  ( -25.98076211353311393, 54.57499999999986073, -7.000000000000072831 ) ) ;
#4457 = CARTESIAN_POINT ( 'NONE',  ( 20.52771519157129987, 16.80080847068802541, 11.95042449705224819 ) ) ;
#4458 = EDGE_CURVE ( 'NONE', #5004, #5575, #2606, .T. ) ;
#4459 = DIRECTION ( 'NONE',  ( 0.000000000000000000, 1.000000000000000000, 0.000000000000000000 ) ) ;
#4460 = ADVANCED_FACE ( 'NONE', ( #356 ), #9384, .T. ) ;
#4461 = CARTESIAN_POINT ( 'NONE',  ( -25.17020516978313083, 52.81041666571061199, -6.403925809002825709 ) ) ;
#4462 = DIRECTION ( 'NONE',  ( 0.000000000000000000, -0.5000000000000011102, -0.8660254037844379305 ) ) ;
#4463 = VERTEX_POINT ( 'NONE', #8552 ) ;
#4464 = LINE ( 'NONE', #6169, #8658 ) ;
#4465 = EDGE_LOOP ( 'NONE', ( #4031, #7377, #5384, #3133 ) ) ;
#4466 = CARTESIAN_POINT ( 'NONE',  ( -1.515916693951010252, 33.47259180932604750, 12.73656658473306358 ) ) ;
#4467 = ORIENTED_EDGE ( 'NONE', *, *, #498, .T. ) ;
#4468 = CARTESIAN_POINT ( 'NONE',  ( 19.36223501247343393, 16.11237126175916501, 11.95718771041564210 ) ) ;
#4469 =( NAMED_UNIT ( * ) SI_UNIT ( $, .STERADIAN. ) SOLID_ANGLE_UNIT ( ) );
#4470 = B_SPLINE_CURVE_WITH_KNOTS ( 'NONE', 3,
 ( #8530, #9358, #2523, #6858, #5091 ),
 .UNSPECIFIED., .F., .F.,
 ( 4, 1, 4 ),
 ( 0.000000000000000000, 0.002309401076758505790, 0.004618802153517011580 ),
 .UNSPECIFIED. ) ;
#4471 = CARTESIAN_POINT ( 'NONE',  ( 22.96512898726170704, 23.28924158689358848, 11.95042449705224819 ) ) ;
#4472 = CARTESIAN_POINT ( 'NONE',  ( 20.17304365239387565, 21.99495017005343200, 12.00579112326981068 ) ) ;
#4473 = VECTOR ( 'NONE', #1761, 999.9999999999998863 ) ;
#4474 = CARTESIAN_POINT ( 'NONE',  ( 2.500000000000000000, 2.357898499370433054, -1.951563910473907981E-15 ) ) ;
#4475 = CARTESIAN_POINT ( 'NONE',  ( -4.000000000000000000, 2.309401076758498483, -0.4999999999999927280 ) ) ;
#4476 = DIRECTION ( 'NONE',  ( 0.000000000000000000, 0.000000000000000000, 1.000000000000000000 ) ) ;
#4477 = ORIENTED_EDGE ( 'NONE', *, *, #8457, .T. ) ;
#4478 = ORIENTED_EDGE ( 'NONE', *, *, #5357, .F. ) ;
#4479 = CARTESIAN_POINT ( 'NONE',  ( 16.11564427137601285, 18.83410319690818824, 12.22072830420661660 ) ) ;
#4480 = CIRCLE ( 'NONE', #9606, 4.499999999999999112 ) ;
#4481 = DIRECTION ( 'NONE',  ( -1.156482317317871478E-16, 0.000000000000000000, 1.000000000000000000 ) ) ;
#4482 = SURFACE_SIDE_STYLE ('',( #1072 ) ) ;
#4483 = CARTESIAN_POINT ( 'NONE',  ( 4.750000000000000888, 3.980102097228896752E-16, -3.249999999999999112 ) ) ;
#4484 = PLANE ( 'NONE',  #4822 ) ;
#4485 = CARTESIAN_POINT ( 'NONE',  ( -25.98076211353311393, 50.63749999808803892, -3.000000000000132339 ) ) ;
#4486 = CARTESIAN_POINT ( 'NONE',  ( 25.98076211353311749, 56.49999999999984368, 7.850000000000012967 ) ) ;
#4487 = CARTESIAN_POINT ( 'NONE',  ( -3.505208318772512488, 29.79067687212226545, 17.48140433884295319 ) ) ;
#4488 = CARTESIAN_POINT ( 'NONE',  ( 3.200000000000006395, -2.686816014504533001, 2.346298152288395666 ) ) ;
#4489 = ADVANCED_FACE ( 'NONE', ( #934 ), #2098, .F. ) ;
#4490 = ORIENTED_EDGE ( 'NONE', *, *, #9950, .T. ) ;
#4491 = DIRECTION ( 'NONE',  ( 1.000000000000000000, 0.000000000000000000, 0.000000000000000000 ) ) ;
#4492 = CARTESIAN_POINT ( 'NONE',  ( -1.101703131577911776, 27.52740819067395250, 15.20093341526694353 ) ) ;
#4493 = CARTESIAN_POINT ( 'NONE',  ( 1.767766952966372429, 31.76776695296637598, 13.50000000000000355 ) ) ;
#4494 = CARTESIAN_POINT ( 'NONE',  ( 29.17190429162963738, 2.000000000000001776, -12.50099999999999767 ) ) ;
#4495 = CARTESIAN_POINT ( 'NONE',  ( 24.50857997860451931, -3.999999999999984457, 10.00000000000000888 ) ) ;
#4496 = CARTESIAN_POINT ( 'NONE',  ( 0.000000000000000000, -2.357898499370432610, 3.252606517456513302E-15 ) ) ;
#4497 = CARTESIAN_POINT ( 'NONE',  ( -24.98076211353312814, 55.21666666666653356, -6.732050807568954909 ) ) ;
#4498 = AXIS2_PLACEMENT_3D ( 'NONE', #4407, #8098, #3926 ) ;
#4499 = ORIENTED_EDGE ( 'NONE', *, *, #7917, .T. ) ;
#4500 = ORIENTED_EDGE ( 'NONE', *, *, #2218, .T. ) ;
#4501 = CARTESIAN_POINT ( 'NONE',  ( 25.00000000000000000, 0.000000000000000000, 0.000000000000000000 ) ) ;
#4502 = CARTESIAN_POINT ( 'NONE',  ( -25.98076211353311393, 49.49999999999986500, -5.000000000000103029 ) ) ;
#4503 = ORIENTED_EDGE ( 'NONE', *, *, #131, .T. ) ;
#4504 = PLANE ( 'NONE',  #5247 ) ;
#4505 = CARTESIAN_POINT ( 'NONE',  ( -27.98076211353308551, 51.92083333142137036, -3.845299461620869330 ) ) ;
#4506 = EDGE_CURVE ( 'NONE', #6542, #318, #408, .T. ) ;
#4507 = CARTESIAN_POINT ( 'NONE',  ( 19.25788680476432546, 17.21053220311310739, 11.00783986014182148 ) ) ;
#4508 = CARTESIAN_POINT ( 'NONE',  ( -24.17020516978314504, 49.60937499952190421, -5.000000000000103029 ) ) ;
#4509 = CARTESIAN_POINT ( 'NONE',  ( -26.79131905728310059, 52.92708333237727913, -6.403925809002825709 ) ) ;
#4510 = PLANE ( 'NONE',  #3948 ) ;
#4511 = ORIENTED_EDGE ( 'NONE', *, *, #9537, .F. ) ;
#4512 = CARTESIAN_POINT ( 'NONE',  ( -25.98076211353311393, 50.98749999808804034, -7.000000000000073719 ) ) ;
#4513 = ORIENTED_EDGE ( 'NONE', *, *, #2602, .F. ) ;
#4514 = CARTESIAN_POINT ( 'NONE',  ( -1.101703131577916883, 32.47259180932605460, 15.23656658473306535 ) ) ;
#4515 = VERTEX_POINT ( 'NONE', #519 ) ;
#4516 = CARTESIAN_POINT ( 'NONE',  ( 23.54706165660595829, 18.96431965174070555, 11.95042449705224819 ) ) ;
#4517 = EDGE_CURVE ( 'NONE', #681, #9108, #8090, .T. ) ;
#4518 = FACE_OUTER_BOUND ( 'NONE', #10135, .T. ) ;
#4519 = ADVANCED_FACE ( 'NONE', ( #4813 ), #1309, .F. ) ;
#4520 = CARTESIAN_POINT ( 'NONE',  ( 22.03595509826854126, 19.06622527062933870, 12.00579112326941988 ) ) ;
#4521 = CARTESIAN_POINT ( 'NONE',  ( -24.35964822603314417, 53.91874999904395338, -5.000000000000103029 ) ) ;
#4522 = CARTESIAN_POINT ( 'NONE',  ( 29.49999999999999645, -3.999999999999986233, -4.999999999999991118 ) ) ;
#4523 = DIRECTION ( 'NONE',  ( 0.000000000000000000, 0.000000000000000000, 1.000000000000000000 ) ) ;
#4524 = CYLINDRICAL_SURFACE ( 'NONE', #7223, 4.500000000000000888 ) ;
#4525 = ORIENTED_EDGE ( 'NONE', *, *, #10248, .F. ) ;
#4526 = PLANE ( 'NONE',  #2785 ) ;
#4527 = EDGE_CURVE ( 'NONE', #7218, #6966, #3188, .T. ) ;
#4528 = DIRECTION ( 'NONE',  ( 0.000000000000000000, 0.000000000000000000, 1.000000000000000000 ) ) ;
#4529 = SURFACE_STYLE_USAGE ( .BOTH. , #7084 ) ;
#4530 = CARTESIAN_POINT ( 'NONE',  ( -25.98076211353311393, 54.22499999999985931, -3.000000000000132339 ) ) ;
#4531 = CIRCLE ( 'NONE', #8611, 24.99999999999999645 ) ;
#4532 = CARTESIAN_POINT ( 'NONE',  ( -26.51666049839535688, 52.41876073720499818, -7.000000000000071942 ) ) ;
#4533 = DIRECTION ( 'NONE',  ( 0.000000000000000000, -0.000000000000000000, -1.000000000000000000 ) ) ;
#4534 = AXIS2_PLACEMENT_3D ( 'NONE', #5281, #3390, #4455 ) ;
#4535 = ADVANCED_FACE ( 'NONE', ( #3965 ), #4081, .F. ) ;
#4536 = EDGE_CURVE ( 'NONE', #7419, #702, #790, .T. ) ;
#4537 =( LENGTH_UNIT ( ) NAMED_UNIT ( * ) SI_UNIT ( .MILLI., .METRE. ) );
#4538 = CARTESIAN_POINT ( 'NONE',  ( -2.428085025993355295, 32.52166244231248271, 17.31030841526694175 ) ) ;
#4539 = DIRECTION ( 'NONE',  ( -0.000000000000000000, -0.000000000000000000, -1.000000000000000000 ) ) ;
#4540 = ORIENTED_EDGE ( 'NONE', *, *, #2856, .T. ) ;
#4541 = DIRECTION ( 'NONE',  ( 0.000000000000000000, 1.000000000000000000, 0.000000000000000000 ) ) ;
#4542 = VECTOR ( 'NONE', #150, 1000.000000000000000 ) ;
#4543 = CARTESIAN_POINT ( 'NONE',  ( -2.500000000000004441, 28.96446609406725159, 15.29687500000000178 ) ) ;
#4544 = CYLINDRICAL_SURFACE ( 'NONE', #2825, 3.000000000000000000 ) ;
#4545 = CIRCLE ( 'NONE', #5774, 1.535500000000000087 ) ;
#4546 = CARTESIAN_POINT ( 'NONE',  ( 20.00651627240589647, 19.97666299463432438, 12.00579112326824216 ) ) ;
#4547 = CARTESIAN_POINT ( 'NONE',  ( -25.98076211353324894, 13.49999999999941913, -2.850000000000009859 ) ) ;
#4548 = ADVANCED_FACE ( 'NONE', ( #2305 ), #10743, .T. ) ;
#4549 = CARTESIAN_POINT ( 'NONE',  ( 29.49999999999999645, -8.499999999999984013, 10.00000000000001243 ) ) ;
#4550 = CIRCLE ( 'NONE', #5609, 5.384454397937118664 ) ;
#4551 = CARTESIAN_POINT ( 'NONE',  ( -25.98076211353311393, 53.91874999904394627, -3.128098921329806714 ) ) ;
#4552 = CARTESIAN_POINT ( 'NONE',  ( 34.99999999999987210, -3.999999999999989786, 9.999999999999998224 ) ) ;
#4553 = CARTESIAN_POINT ( 'NONE',  ( -27.98076211353308551, 55.44999999999986073, -5.000000000000103029 ) ) ;
#4554 = VECTOR ( 'NONE', #4539, 1000.000000000000000 ) ;
#4555 = EDGE_LOOP ( 'NONE', ( #5712, #1675, #7667 ) ) ;
#4556 = ORIENTED_EDGE ( 'NONE', *, *, #1898, .T. ) ;
#4557 = DIRECTION ( 'NONE',  ( 0.000000000000000000, 1.000000000000000000, 0.000000000000000000 ) ) ;
#4558 = LINE ( 'NONE', #6992, #6634 ) ;
#4559 = ORIENTED_EDGE ( 'NONE', *, *, #9566, .T. ) ;
#4560 = DIRECTION ( 'NONE',  ( 0.000000000000000000, -0.4999999999999991118, 0.8660254037844391517 ) ) ;
#4561 = AXIS2_PLACEMENT_3D ( 'NONE', #5641, #3803, #514 ) ;
#4562 = DIRECTION ( 'NONE',  ( 0.000000000000000000, -0.7071067811865420216, -0.7071067811865531239 ) ) ;
#4563 = CARTESIAN_POINT ( 'NONE',  ( 17.74785087444460885, 17.25574343990722070, 11.06843699004799397 ) ) ;
#4564 = ORIENTED_EDGE ( 'NONE', *, *, #8797, .T. ) ;
#4565 = CARTESIAN_POINT ( 'NONE',  ( -27.60187600103308014, 51.58541666571061768, -5.935950539335252074 ) ) ;
#4566 = VERTEX_POINT ( 'NONE', #6515 ) ;
#4567 = DIRECTION ( 'NONE',  ( 0.000000000000000000, 0.000000000000000000, 1.000000000000000000 ) ) ;
#4568 = ORIENTED_EDGE ( 'NONE', *, *, #3686, .F. ) ;
#4569 = CARTESIAN_POINT ( 'NONE',  ( -2.494791681227495950, 29.73705052183845154, 15.48578750830907147 ) ) ;
#4570 = ORIENTED_EDGE ( 'NONE', *, *, #6544, .F. ) ;
#4571 = ADVANCED_FACE ( 'NONE', ( #6370 ), #8427, .F. ) ;
#4572 = CARTESIAN_POINT ( 'NONE',  ( 24.04035011313704118, 22.03839429810881612, 10.95195840513898666 ) ) ;
#4573 =( BOUNDED_SURFACE ( )  B_SPLINE_SURFACE ( 1, 2, ( 
 ( #9997, #9272, #47, #3451, #1666, #10883, #6830, #5065, #8443, #822, #10225, #3275, #7728, #6658, #106, #10652, #7991, #4769, #8148, #8040, #1989, #4608, #5544, #5435, #1313, #2833, #3815, #9706, #2102, #4712, #6254, #5495, #7203, #7148, #2041, #9763, #6315, #8759, #10279, #1204, #8879, #10598, #10542, #1264, #9647, #2938, #8822, #4658, #413, #6374, #3709, #8981, #362, #3765, #2199, #2995, #2153, #6204, #8925, #8093, #470, #5375, #3872, #7256, #3042, #6416, #9814, #5595, #1142, #4551, #1371, #523, #6893, #9588, #7935, #313, #10491, #7099, #2882, #5863, #9191, #10807, #1642, #687, #9923, #7470, #9245, #10031, #4869, #8303, #2420, #2310, #4086, #9034, #2359, #6693, #1585, #8248, #10860, #3250, #4983, #9079, #4931, #5749, #9974 ),
 ( #4027, #10748, #6624, #3921, #3192, #5805, #8357, #7360, #8412, #736, #3969, #634, #5701, #7415, #7306, #6573, #6468, #9134, #7527, #1530, #5037, #10698, #4137, #9869, #1475, #10917, #3309, #10090, #3091, #2479, #2258, #5652, #1425, #3140, #4818, #8196, #574, #6520, #10196, #6921, #2758, #9527, #10362, #6862, #5153, #9414, #1927, #859, #6801, #6134, #6081, #8475, #1698, #5314, #795, #4199, #10255, #8534, #1812, #7589, #4260, #2595, #10979, #9470, #7645, #5095, #5206, #3367, #9364, #3539, #2655, #7758, #22, #1023, #3424, #8583, #966, #2705, #6030, #4373, #1863, #6747, #2531, #139, #5974, #5916, #9299, #3482, #10310, #1762, #911, #5259, #10144, #8642, #4435, #4314, #7701, #7817, #189, #77, #3590, #6974, #8747, #10530, #1129 ) ),
 .UNSPECIFIED., .F., .F., .T. ) 
 B_SPLINE_SURFACE_WITH_KNOTS ( ( 2, 2 ),
 ( 3, 2, 2, 2, 2, 2, 2, 2, 2, 2, 2, 2, 2, 2, 2, 2, 2, 2, 2, 2, 2, 2, 2, 2, 2, 2, 2, 2, 2, 2, 2, 2, 2, 2, 2, 2, 2, 2, 2, 2, 2, 2, 2, 2, 2, 2, 2, 2, 2, 2, 2, 2, 3 ),
 ( 0.000000000000000000, 1.000000000000000000 ),
 ( 0.000000000000000000, 0.01851851851851851749, 0.03703703703703703498, 0.05555555555555555247, 0.07407407407407406996, 0.09259259259259258745, 0.1111111111111111049, 0.1296296296296296224, 0.1481481481481481399, 0.1666666666666666574, 0.1851851851851851749, 0.2037037037037036924, 0.2222222222222222099, 0.2407407407407407274, 0.2592592592592592449, 0.2777777777777777901, 0.2962962962962962798, 0.3148148148148148251, 0.3333333333333333148, 0.3518518518518518601, 0.3703703703703703498, 0.3888888888888888951, 0.4074074074074073848, 0.4259259259259259300, 0.4444444444444444198, 0.4629629629629629650, 0.4814814814814814548, 0.5000000000000000000, 0.5185185185185184897, 0.5370370370370370905, 0.5555555555555555802, 0.5740740740740740700, 0.5925925925925925597, 0.6111111111111111605, 0.6296296296296296502, 0.6481481481481481399, 0.6666666666666666297, 0.6851851851851852304, 0.7037037037037037202, 0.7222222222222222099, 0.7407407407407406996, 0.7592592592592593004, 0.7777777777777777901, 0.7962962962962962798, 0.8148148148148147696, 0.8333333333333333703, 0.8518518518518518601, 0.8703703703703703498, 0.8888888888888888395, 0.9074074074074074403, 0.9259259259259259300, 0.9444444444444444198, 0.9524110019551522699 ),
 .UNSPECIFIED. ) 
 GEOMETRIC_REPRESENTATION_ITEM ( )  RATIONAL_B_SPLINE_SURFACE ( (
 ( 1.000000000000000000, 0.8660254037844387076, 1.000000000000000000, 0.8660254037844387076, 1.000000000000000000, 0.8660254037844387076, 1.000000000000000000, 0.8660254037844387076, 1.000000000000000000, 0.8660254037844387076, 1.000000000000000000, 0.8660254037844387076, 1.000000000000000000, 0.8660254037844387076, 1.000000000000000000, 0.8660254037844387076, 1.000000000000000000, 0.8660254037844387076, 1.000000000000000000, 0.8660254037844387076, 1.000000000000000000, 0.8660254037844387076, 1.000000000000000000, 0.8660254037844387076, 1.000000000000000000, 0.8660254037844387076, 1.000000000000000000, 0.8660254037844387076, 1.000000000000000000, 0.8660254037844387076, 1.000000000000000000, 0.8660254037844387076, 1.000000000000000000, 0.8660254037844387076, 1.000000000000000000, 0.8660254037844387076, 1.000000000000000000, 0.8660254037844387076, 1.000000000000000000, 0.8660254037844387076, 1.000000000000000000, 0.8660254037844387076, 1.000000000000000000, 0.8660254037844387076, 1.000000000000000000, 0.8660254037844387076, 1.000000000000000000, 0.8660254037844387076, 1.000000000000000000, 0.8660254037844387076, 1.000000000000000000, 0.8660254037844387076, 1.000000000000000000, 0.8660254037844387076, 1.000000000000000000, 0.8660254037844387076, 1.000000000000000000, 0.8660254037844387076, 1.000000000000000000, 0.8660254037844387076, 1.000000000000000000, 0.8660254037844387076, 1.000000000000000000, 0.8660254037844387076, 1.000000000000000000, 0.8660254037844387076, 1.000000000000000000, 0.8660254037844387076, 1.000000000000000000, 0.8660254037844387076, 1.000000000000000000, 0.8660254037844387076, 1.000000000000000000, 0.8660254037844387076, 1.000000000000000000, 0.8660254037844387076, 1.000000000000000000, 0.8660254037844387076, 1.000000000000000000, 0.8660254037844387076, 1.000000000000000000, 0.8660254037844387076, 1.000000000000000000, 0.8660254037844387076, 1.000000000000000000, 0.8660254037844387076, 1.000000000000000000, 0.8660254037844387076, 1.000000000000000000, 0.8660254037844387076, 1.000000000000000000, 0.8660254037844387076, 1.000000000000000000, 0.8660254037844387076, 1.000000000000000000, 0.8660254037844387076, 1.000000000000000000, 0.8660254037844387076, 1.000000000000000000, 0.8660254037844387076, 1.000000000000000000, 0.8660254037844387076, 1.000000000000000000, 0.9423649184108428001, 0.9343183815700366601),
 ( 1.000000000000000000, 0.8660254037844387076, 1.000000000000000000, 0.8660254037844387076, 1.000000000000000000, 0.8660254037844387076, 1.000000000000000000, 0.8660254037844387076, 1.000000000000000000, 0.8660254037844387076, 1.000000000000000000, 0.8660254037844387076, 1.000000000000000000, 0.8660254037844387076, 1.000000000000000000, 0.8660254037844387076, 1.000000000000000000, 0.8660254037844387076, 1.000000000000000000, 0.8660254037844387076, 1.000000000000000000, 0.8660254037844387076, 1.000000000000000000, 0.8660254037844387076, 1.000000000000000000, 0.8660254037844387076, 1.000000000000000000, 0.8660254037844387076, 1.000000000000000000, 0.8660254037844387076, 1.000000000000000000, 0.8660254037844387076, 1.000000000000000000, 0.8660254037844387076, 1.000000000000000000, 0.8660254037844387076, 1.000000000000000000, 0.8660254037844387076, 1.000000000000000000, 0.8660254037844387076, 1.000000000000000000, 0.8660254037844387076, 1.000000000000000000, 0.8660254037844387076, 1.000000000000000000, 0.8660254037844387076, 1.000000000000000000, 0.8660254037844387076, 1.000000000000000000, 0.8660254037844387076, 1.000000000000000000, 0.8660254037844387076, 1.000000000000000000, 0.8660254037844387076, 1.000000000000000000, 0.8660254037844387076, 1.000000000000000000, 0.8660254037844387076, 1.000000000000000000, 0.8660254037844387076, 1.000000000000000000, 0.8660254037844387076, 1.000000000000000000, 0.8660254037844387076, 1.000000000000000000, 0.8660254037844387076, 1.000000000000000000, 0.8660254037844387076, 1.000000000000000000, 0.8660254037844387076, 1.000000000000000000, 0.8660254037844387076, 1.000000000000000000, 0.8660254037844387076, 1.000000000000000000, 0.8660254037844387076, 1.000000000000000000, 0.8660254037844387076, 1.000000000000000000, 0.8660254037844387076, 1.000000000000000000, 0.8660254037844387076, 1.000000000000000000, 0.8660254037844387076, 1.000000000000000000, 0.8660254037844387076, 1.000000000000000000, 0.8660254037844387076, 1.000000000000000000, 0.8660254037844387076, 1.000000000000000000, 0.8660254037844387076, 1.000000000000000000, 0.8660254037844387076, 1.000000000000000000, 0.8660254037844387076, 1.000000000000000000, 0.8660254037844387076, 1.000000000000000000, 0.8660254037844387076, 1.000000000000000000, 0.8660254037844387076, 1.000000000000000000, 0.9423649184108428001, 0.9343183815700366601) ) ) 
 REPRESENTATION_ITEM ( '' )  SURFACE ( )  );
#4574 = DIRECTION ( 'NONE',  ( 1.000000000000000000, -0.000000000000000000, 1.156482317317871478E-16 ) ) ;
#4575 = CARTESIAN_POINT ( 'NONE',  ( 23.22159451225019566, 21.65168511467167889, 13.00425721518366728 ) ) ;
#4576 = CARTESIAN_POINT ( 'NONE',  ( -25.98076211353311393, 55.49374999904395622, -6.871901078670400231 ) ) ;
#4577 = SURFACE_STYLE_USAGE ( .BOTH. , #1175 ) ;
#4578 = CIRCLE ( 'NONE', #9893, 0.2000000000000000944 ) ;
#4579 = AXIS2_PLACEMENT_3D ( 'NONE', #284, #10401, #8627 ) ;
#4580 = CARTESIAN_POINT ( 'NONE',  ( -2.345747346278108214, 3.264484291692489215, -0.01223254789873409049 ) ) ;
#4581 = DIRECTION ( 'NONE',  ( 0.000000000000000000, 0.000000000000000000, 1.000000000000000000 ) ) ;
#4582 = EDGE_CURVE ( 'NONE', #10904, #7860, #9919, .T. ) ;
#4583 = VERTEX_POINT ( 'NONE', #5696 ) ;
#4584 = ORIENTED_EDGE ( 'NONE', *, *, #6745, .F. ) ;
#4585 = EDGE_CURVE ( 'NONE', #143, #9227, #9495, .T. ) ;
#4586 = DIRECTION ( 'NONE',  ( -1.000000000000000000, -6.098637220230963674E-17, 0.000000000000000000 ) ) ;
#4587 = CARTESIAN_POINT ( 'NONE',  ( -23.98076211353314235, 50.14166666666653072, -3.845299461620867554 ) ) ;
#4588 = DIRECTION ( 'NONE',  ( -1.000000000000000000, 0.000000000000000000, 0.000000000000000000 ) ) ;
#4589 = VECTOR ( 'NONE', #4374, 1000.000000000000000 ) ;
#4590 = DIRECTION ( 'NONE',  ( -0.000000000000000000, 0.000000000000000000, 1.000000000000000000 ) ) ;
#4591 = CARTESIAN_POINT ( 'NONE',  ( -25.98076211353311393, 52.38749999808802471, -7.000000000000072831 ) ) ;
#4592 = CARTESIAN_POINT ( 'NONE',  ( 21.21106610644839208, 53.49999999999983658, 10.00000000000000178 ) ) ;
#4593 = APPLICATION_CONTEXT ( 'automotive_design' ) ;
#4594 =( NAMED_UNIT ( * ) SI_UNIT ( $, .STERADIAN. ) SOLID_ANGLE_UNIT ( ) );
#4595 = CARTESIAN_POINT ( 'NONE',  ( -3.456897879362375470, 29.45240795142740353, 16.49922112211940117 ) ) ;
#4596 = CARTESIAN_POINT ( 'NONE',  ( -0.6937372685066653943, 4.453844082567723461, -3.610536846335889116 ) ) ;
#4597 = EDGE_CURVE ( 'NONE', #3494, #7883, #1471, .T. ) ;
#4598 = VERTEX_POINT ( 'NONE', #10694 ) ;
#4599 = DIRECTION ( 'NONE',  ( -1.000000000000000000, -0.000000000000000000, -0.000000000000000000 ) ) ;
#4600 = ADVANCED_FACE ( 'NONE', ( #9809 ), #5246, .F. ) ;
#4601 = VECTOR ( 'NONE', #744, 1000.000000000000114 ) ;
#4602 = CARTESIAN_POINT ( 'NONE',  ( -2.472591809326051937, 31.10170313157791000, 16.13843341526694530 ) ) ;
#4603 = CARTESIAN_POINT ( 'NONE',  ( -2.500000000000004441, 28.96446609406725159, 14.04687500000000355 ) ) ;
#4604 = CARTESIAN_POINT ( 'NONE',  ( -25.98076211353311038, 60.99999999999985789, -5.000000000000102141 ) ) ;
#4605 = CARTESIAN_POINT ( 'NONE',  ( -24.98076211353312814, 55.12916666475470606, -6.732050807568954909 ) ) ;
#4606 = DIRECTION ( 'NONE',  ( 0.000000000000000000, 0.000000000000000000, 1.000000000000000000 ) ) ;
#4607 = CARTESIAN_POINT ( 'NONE',  ( 24.55500000000002103, 0.000000000000000000, 0.000000000000000000 ) ) ;
#4608 = CARTESIAN_POINT ( 'NONE',  ( -25.98076211353311393, 51.11874999904394201, -3.128098921329806714 ) ) ;
#4609 = CARTESIAN_POINT ( 'NONE',  ( 2.000000000000000000, 0.8865213383406680414, -1.535500000000000975 ) ) ;
#4610 = CARTESIAN_POINT ( 'NONE',  ( 30.75045812061784289, 53.49999999999983658, 2.500000000000000000 ) ) ;
#4611 = ORIENTED_EDGE ( 'NONE', *, *, #9114, .T. ) ;
#4612 = EDGE_LOOP ( 'NONE', ( #5221, #379, #5238, #1445 ) ) ;
#4613 = DIRECTION ( 'NONE',  ( 1.000000000000000000, 0.000000000000000000, 0.000000000000000000 ) ) ;
#4614 = CYLINDRICAL_SURFACE ( 'NONE', #2751, 1.999999999999971356 ) ;
#4615 = ITEM_DEFINED_TRANSFORMATION ( 'NONE', 'NONE', #1542,  #308 ) ;
#4616 = VERTEX_POINT ( 'NONE', #9969 ) ;
#4617 = DIRECTION ( 'NONE',  ( 0.000000000000000000, 1.000000000000000000, 0.000000000000000000 ) ) ;
#4618 = CARTESIAN_POINT ( 'NONE',  ( -27.60187600103308725, 50.12708333237728198, -4.064049460664955760 ) ) ;
#4619 = CARTESIAN_POINT ( 'NONE',  ( 18.92159813099251053, 21.64660971755233732, 10.95195840513820151 ) ) ;
#4620 = ORIENTED_EDGE ( 'NONE', *, *, #8319, .T. ) ;
#4621 = CARTESIAN_POINT ( 'NONE',  ( -25.17020516978313083, 54.67708333237727913, -3.596074190997380349 ) ) ;
#4622 = ORIENTED_EDGE ( 'NONE', *, *, #1402, .T. ) ;
#4623 = CARTESIAN_POINT ( 'NONE',  ( 2.500000000000000000, 0.000000000000000000, 0.000000000000000000 ) ) ;
#4624 =( BOUNDED_SURFACE ( )  B_SPLINE_SURFACE ( 3, 3, ( 
 ( #951, #5301, #8569, #6117, #2802, #7688, #8628, #61, #7014, #896, #2743, #4298, #3466, #9568, #10241, #8519, #5958, #1118, #5188, #122, #1007, #3406, #9347, #1966, #5350, #10402, #9455, #8734, #2640, #8686, #4520, #3523, #7804, #5, #6909, #4355, #10296, #3574, #6787, #6847, #6959, #9511, #10347, #1061, #10182, #2576, #1744, #2690, #4472, #6016, #5139, #3624, #9401, #1799 ),
 ( #6065, #10673, #9619, #4631, #3790, #10516, #1344, #1172, #1291, #8015, #9841, #8850, #8061, #387, #4685, #7173, #2232, #1234, #443, #10569, #2968, #2130, #7121, #7229, #10626, #9010, #2910, #5404, #2176, #2014, #285, #6279, #4744, #7279, #502, #6341, #2071, #1401, #9677, #9735, #8119, #4575, #3898, #8951, #3019, #5517, #2858, #8899, #7908, #5459, #3843, #7075, #3065, #6394 ),
 ( #3681, #9785, #5624, #5571, #6440, #10464, #6228, #8789, #7961, #338, #3734, #6722, #3220, #4062, #4960, #4843, #760, #6552, #8217, #2449, #9999, #9104, #4164, #10719, #3117, #2501, #2386, #3336, #661, #5777, #546, #4795, #2334, #7444, #9161, #1500, #4901, #10115, #3276, #1557, #1612, #6599, #1450, #2288, #3946, #8331, #5888, #602, #8276, #9274, #10835, #6659, #710, #4111 ),
 ( #7498, #8171, #5010, #10885, #10060, #5836, #7331, #9219, #8385, #6495, #5676, #9897, #7558, #9055, #9949, #10943, #3998, #7388, #10779, #3169, #5727, #6833, #1836, #4457, #3392, #9388, #8556, #4283, #6102, #5944, #3452, #5124, #10334, #6894, #6001, #8673, #7618, #6358, #10389, #10281, #212, #939, #2677, #8445, #1667, #10226, #4339, #6052, #1786, #5175, #6998, #164, #9440, #9497 ),
 ( #10172, #824, #5229, #2788, #9332, #7729, #3611, #109, #3561, #3507, #8614, #994, #4403, #7790, #6163, #1897, #6944, #2729, #5284, #5066, #1048, #7839, #4229, #2560, #6773, #1726, #8502, #2622, #882, #7673, #48, #2118, #2951, #425, #3722, #9719, #1328, #271, #6265, #5447, #1159, #3006, #2846, #6326, #9660, #485, #10506, #5505, #2057, #4619, #3778, #8773, #8888, #1278 ),
 ( #7060, #3830, #3668, #1955, #7949, #6384, #8936, #2164, #2897, #7110, #3054, #4563, #8836, #9773, #6217, #5556, #10611, #4670, #7159, #4507, #10553, #9555, #327, #8049, #8720, #4728, #7215, #8105, #5336, #1102, #1222, #3884, #7267, #8004, #10662, #375, #7892, #10451, #9602, #2000, #5388, #4881, #5710, #6581, #6480, #2429, #2272, #5663, #9984, #6536, #9933, #4781, #5612, #2368 ),
 ( #10928, #1434, #5761, #8994, #9203, #9145, #1540, #2215, #6428, #9089, #8367, #696, #4830, #1596, #8261, #3259, #1385, #3102, #8159, #746, #644, #1483, #4945, #9881, #5821, #8205, #9042, #4095, #4043, #10760, #4994, #534, #3933, #4146, #7427, #7539, #2318, #10817, #7318, #9827, #3981, #3202, #8314, #3153, #7482, #10706, #10870, #6640, #10044, #585, #7375, #807, #2488, #92 ) ),
 .UNSPECIFIED., .T., .F., .F. ) 
 B_SPLINE_SURFACE_WITH_KNOTS ( ( 4, 3, 4 ),
 ( 4, 2, 2, 2, 2, 2, 2, 2, 2, 2, 2, 2, 2, 2, 2, 2, 2, 2, 2, 2, 2, 2, 2, 2, 2, 2, 4 ),
 ( 0.000000000000000000, 0.5000000000000000000, 1.000000000000000000 ),
 ( 0.000000000000000000, 0.05059550242166081097, 0.08415034466705637040, 0.1009277657897541536, 0.1177051869124519229, 0.1353321994541143436, 0.1529592119957767782, 0.1882132370791016474, 0.2234672621624265165, 0.2410942747040889511, 0.2587212872457513857, 0.2827395206004625905, 0.3067577539551737398, 0.3547942206645960939, 0.4028306873740183924, 0.4268489207287295972, 0.4508671540834407465, 0.4680275555183331937, 0.4851879569532256964, 0.5195087598230107018, 0.5881503655625806015, 0.6567919713021505013, 0.7254335770417204010, 0.7940751827812903008, 0.8627167885208602005, 0.9313583942604301003, 1.000000000000000000 ),
 .UNSPECIFIED. ) 
 GEOMETRIC_REPRESENTATION_ITEM ( )  RATIONAL_B_SPLINE_SURFACE ( (
 ( 1.000000000000000000, 1.000000000000000000, 1.000000000000000000, 1.000000000000000000, 1.000000000000000000, 1.000000000000000000, 1.000000000000000000, 1.000000000000000000, 1.000000000000000000, 1.000000000000000000, 1.000000000000000000, 1.000000000000000000, 1.000000000000000000, 1.000000000000000000, 1.000000000000000000, 1.000000000000000000, 1.000000000000000000, 1.000000000000000000, 1.000000000000000000, 1.000000000000000000, 1.000000000000000000, 1.000000000000000000, 1.000000000000000000, 1.000000000000000000, 1.000000000000000000, 1.000000000000000000, 1.000000000000000000, 1.000000000000000000, 1.000000000000000000, 1.000000000000000000, 1.000000000000000000, 1.000000000000000000, 1.000000000000000000, 1.000000000000000000, 1.000000000000000000, 1.000000000000000000, 1.000000000000000000, 1.000000000000000000, 1.000000000000000000, 1.000000000000000000, 1.000000000000000000, 1.000000000000000000, 1.000000000000000000, 1.000000000000000000, 1.000000000000000000, 1.000000000000000000, 1.000000000000000000, 1.000000000000000000, 1.000000000000000000, 1.000000000000000000, 1.000000000000000000, 1.000000000000000000, 1.000000000000000000, 1.000000000000000000),
 ( 0.3333333333333333703, 0.3333333333333333703, 0.3333333333333333703, 0.3333333333333333703, 0.3333333333333333703, 0.3333333333333333703, 0.3333333333333333703, 0.3333333333333333703, 0.3333333333333333703, 0.3333333333333333703, 0.3333333333333333703, 0.3333333333333333703, 0.3333333333333333703, 0.3333333333333333703, 0.3333333333333333703, 0.3333333333333333703, 0.3333333333333333703, 0.3333333333333333703, 0.3333333333333333703, 0.3333333333333333703, 0.3333333333333333703, 0.3333333333333333703, 0.3333333333333333703, 0.3333333333333333703, 0.3333333333333333703, 0.3333333333333333703, 0.3333333333333333703, 0.3333333333333333703, 0.3333333333333333703, 0.3333333333333333703, 0.3333333333333333703, 0.3333333333333333703, 0.3333333333333333703, 0.3333333333333333703, 0.3333333333333333703, 0.3333333333333333703, 0.3333333333333333703, 0.3333333333333333703, 0.3333333333333333703, 0.3333333333333333703, 0.3333333333333333703, 0.3333333333333333703, 0.3333333333333333703, 0.3333333333333333703, 0.3333333333333333703, 0.3333333333333333703, 0.3333333333333333703, 0.3333333333333333703, 0.3333333333333333703, 0.3333333333333333703, 0.3333333333333333703, 0.3333333333333333703, 0.3333333333333333703, 0.3333333333333333703),
 ( 0.3333333333333333703, 0.3333333333333333703, 0.3333333333333333703, 0.3333333333333333703, 0.3333333333333333703, 0.3333333333333333703, 0.3333333333333333703, 0.3333333333333333703, 0.3333333333333333703, 0.3333333333333333703, 0.3333333333333333703, 0.3333333333333333703, 0.3333333333333333703, 0.3333333333333333703, 0.3333333333333333703, 0.3333333333333333703, 0.3333333333333333703, 0.3333333333333333703, 0.3333333333333333703, 0.3333333333333333703, 0.3333333333333333703, 0.3333333333333333703, 0.3333333333333333703, 0.3333333333333333703, 0.3333333333333333703, 0.3333333333333333703, 0.3333333333333333703, 0.3333333333333333703, 0.3333333333333333703, 0.3333333333333333703, 0.3333333333333333703, 0.3333333333333333703, 0.3333333333333333703, 0.3333333333333333703, 0.3333333333333333703, 0.3333333333333333703, 0.3333333333333333703, 0.3333333333333333703, 0.3333333333333333703, 0.3333333333333333703, 0.3333333333333333703, 0.3333333333333333703, 0.3333333333333333703, 0.3333333333333333703, 0.3333333333333333703, 0.3333333333333333703, 0.3333333333333333703, 0.3333333333333333703, 0.3333333333333333703, 0.3333333333333333703, 0.3333333333333333703, 0.3333333333333333703, 0.3333333333333333703, 0.3333333333333333703),
 ( 1.000000000000000000, 1.000000000000000000, 1.000000000000000000, 1.000000000000000000, 1.000000000000000000, 1.000000000000000000, 1.000000000000000000, 1.000000000000000000, 1.000000000000000000, 1.000000000000000000, 1.000000000000000000, 1.000000000000000000, 1.000000000000000000, 1.000000000000000000, 1.000000000000000000, 1.000000000000000000, 1.000000000000000000, 1.000000000000000000, 1.000000000000000000, 1.000000000000000000, 1.000000000000000000, 1.000000000000000000, 1.000000000000000000, 1.000000000000000000, 1.000000000000000000, 1.000000000000000000, 1.000000000000000000, 1.000000000000000000, 1.000000000000000000, 1.000000000000000000, 1.000000000000000000, 1.000000000000000000, 1.000000000000000000, 1.000000000000000000, 1.000000000000000000, 1.000000000000000000, 1.000000000000000000, 1.000000000000000000, 1.000000000000000000, 1.000000000000000000, 1.000000000000000000, 1.000000000000000000, 1.000000000000000000, 1.000000000000000000, 1.000000000000000000, 1.000000000000000000, 1.000000000000000000, 1.000000000000000000, 1.000000000000000000, 1.000000000000000000, 1.000000000000000000, 1.000000000000000000, 1.000000000000000000, 1.000000000000000000),
 ( 0.3333333333333333703, 0.3333333333333333703, 0.3333333333333333703, 0.3333333333333333703, 0.3333333333333333703, 0.3333333333333333703, 0.3333333333333333703, 0.3333333333333333703, 0.3333333333333333703, 0.3333333333333333703, 0.3333333333333333703, 0.3333333333333333703, 0.3333333333333333703, 0.3333333333333333703, 0.3333333333333333703, 0.3333333333333333703, 0.3333333333333333703, 0.3333333333333333703, 0.3333333333333333703, 0.3333333333333333703, 0.3333333333333333703, 0.3333333333333333703, 0.3333333333333333703, 0.3333333333333333703, 0.3333333333333333703, 0.3333333333333333703, 0.3333333333333333703, 0.3333333333333333703, 0.3333333333333333703, 0.3333333333333333703, 0.3333333333333333703, 0.3333333333333333703, 0.3333333333333333703, 0.3333333333333333703, 0.3333333333333333703, 0.3333333333333333703, 0.3333333333333333703, 0.3333333333333333703, 0.3333333333333333703, 0.3333333333333333703, 0.3333333333333333703, 0.3333333333333333703, 0.3333333333333333703, 0.3333333333333333703, 0.3333333333333333703, 0.3333333333333333703, 0.3333333333333333703, 0.3333333333333333703, 0.3333333333333333703, 0.3333333333333333703, 0.3333333333333333703, 0.3333333333333333703, 0.3333333333333333703, 0.3333333333333333703),
 ( 0.3333333333333333703, 0.3333333333333333703, 0.3333333333333333703, 0.3333333333333333703, 0.3333333333333333703, 0.3333333333333333703, 0.3333333333333333703, 0.3333333333333333703, 0.3333333333333333703, 0.3333333333333333703, 0.3333333333333333703, 0.3333333333333333703, 0.3333333333333333703, 0.3333333333333333703, 0.3333333333333333703, 0.3333333333333333703, 0.3333333333333333703, 0.3333333333333333703, 0.3333333333333333703, 0.3333333333333333703, 0.3333333333333333703, 0.3333333333333333703, 0.3333333333333333703, 0.3333333333333333703, 0.3333333333333333703, 0.3333333333333333703, 0.3333333333333333703, 0.3333333333333333703, 0.3333333333333333703, 0.3333333333333333703, 0.3333333333333333703, 0.3333333333333333703, 0.3333333333333333703, 0.3333333333333333703, 0.3333333333333333703, 0.3333333333333333703, 0.3333333333333333703, 0.3333333333333333703, 0.3333333333333333703, 0.3333333333333333703, 0.3333333333333333703, 0.3333333333333333703, 0.3333333333333333703, 0.3333333333333333703, 0.3333333333333333703, 0.3333333333333333703, 0.3333333333333333703, 0.3333333333333333703, 0.3333333333333333703, 0.3333333333333333703, 0.3333333333333333703, 0.3333333333333333703, 0.3333333333333333703, 0.3333333333333333703),
 ( 1.000000000000000000, 1.000000000000000000, 1.000000000000000000, 1.000000000000000000, 1.000000000000000000, 1.000000000000000000, 1.000000000000000000, 1.000000000000000000, 1.000000000000000000, 1.000000000000000000, 1.000000000000000000, 1.000000000000000000, 1.000000000000000000, 1.000000000000000000, 1.000000000000000000, 1.000000000000000000, 1.000000000000000000, 1.000000000000000000, 1.000000000000000000, 1.000000000000000000, 1.000000000000000000, 1.000000000000000000, 1.000000000000000000, 1.000000000000000000, 1.000000000000000000, 1.000000000000000000, 1.000000000000000000, 1.000000000000000000, 1.000000000000000000, 1.000000000000000000, 1.000000000000000000, 1.000000000000000000, 1.000000000000000000, 1.000000000000000000, 1.000000000000000000, 1.000000000000000000, 1.000000000000000000, 1.000000000000000000, 1.000000000000000000, 1.000000000000000000, 1.000000000000000000, 1.000000000000000000, 1.000000000000000000, 1.000000000000000000, 1.000000000000000000, 1.000000000000000000, 1.000000000000000000, 1.000000000000000000, 1.000000000000000000, 1.000000000000000000, 1.000000000000000000, 1.000000000000000000, 1.000000000000000000, 1.000000000000000000) ) ) 
 REPRESENTATION_ITEM ( '' )  SURFACE ( )  );
#4625 = ORIENTED_EDGE ( 'NONE', *, *, #6854, .F. ) ;
#4626 = CARTESIAN_POINT ( 'NONE',  ( -0.06616922564517727090, 32.50000000000000711, 13.90844158473306713 ) ) ;
#4627 = ORIENTED_EDGE ( 'NONE', *, *, #5270, .F. ) ;
#4628 = CARTESIAN_POINT ( 'NONE',  ( 15.83366986443827962, 19.11607760386789323, 11.24497629747462568 ) ) ;
#4629 = FILL_AREA_STYLE_COLOUR ( '', #1208 ) ;
#4630 = DIRECTION ( 'NONE',  ( 1.000000000000000000, 0.000000000000000000, 0.000000000000000000 ) ) ;
#4631 = CARTESIAN_POINT ( 'NONE',  ( 16.78877909162549642, 18.16096837667994279, 13.15979613361243494 ) ) ;
#4632 = CARTESIAN_POINT ( 'NONE',  ( -25.98076211353311393, 54.09374999904395054, -6.871901078670400231 ) ) ;
#4633 = DIRECTION ( 'NONE',  ( -0.000000000000000000, -0.000000000000000000, -1.000000000000000000 ) ) ;
#4634 = LINE ( 'NONE', #2076, #1010 ) ;
#4635 = VERTEX_POINT ( 'NONE', #5745 ) ;
#4636 = ORIENTED_EDGE ( 'NONE', *, *, #743, .F. ) ;
#4637 = CARTESIAN_POINT ( 'NONE',  ( 23.33980466280999977, 20.94445964013513617, 12.00579112326902909 ) ) ;
#4638 = DIRECTION ( 'NONE',  ( -0.000000000000000000, 0.000000000000000000, 1.000000000000000000 ) ) ;
#4639 = CARTESIAN_POINT ( 'NONE',  ( -25.98076211353311393, 50.37499999999987210, -7.000000000000073719 ) ) ;
#4640 = CARTESIAN_POINT ( 'NONE',  ( -26.59846429743006269, 58.79685839844216133, -3.095304781643430925 ) ) ;
#4641 = CARTESIAN_POINT ( 'NONE',  ( 0.000000000000000000, 0.8865213383406680414, -1.535500000000000975 ) ) ;
#4642 = LINE ( 'NONE', #7290, #6230 ) ;
#4643 = CARTESIAN_POINT ( 'NONE',  ( -25.98076211353311038, 49.67499999999986215, -7.000000000000072831 ) ) ;
#4644 = CARTESIAN_POINT ( 'NONE',  ( -3.467250377026234176, 29.51776231023078623, 17.49702953738633937 ) ) ;
#4645 = FACE_OUTER_BOUND ( 'NONE', #1478, .T. ) ;
#4646 = EDGE_LOOP ( 'NONE', ( #6823, #7487 ) ) ;
#4647 = CARTESIAN_POINT ( 'NONE',  ( 29.49999999999999645, 2.000000000000001776, -12.49999999999999822 ) ) ;
#4648 = B_SPLINE_CURVE_WITH_KNOTS ( 'NONE', 3,
 ( #7401, #6562, #8288, #8344, #676, #4073 ),
 .UNSPECIFIED., .F., .F.,
 ( 4, 2, 4 ),
 ( 0.002365888236227977302, 0.003551327329835078910, 0.004736766423442180518 ),
 .UNSPECIFIED. ) ;
#4649 = AXIS2_PLACEMENT_3D ( 'NONE', #10961, #3235, #6676 ) ;
#4650 = CARTESIAN_POINT ( 'NONE',  ( 3.527408190673964494, 31.38357824266065776, 15.66968341526694175 ) ) ;
#4651 = CARTESIAN_POINT ( 'NONE',  ( -0.9693646802875689472, 32.52740819067395961, 17.23218341526694530 ) ) ;
#4652 = DIRECTION ( 'NONE',  ( 1.156482317317871725E-16, -2.312964634635742464E-16, -1.000000000000000000 ) ) ;
#4653 = DIRECTION ( 'NONE',  ( -6.098637220230963674E-17, 1.000000000000000000, 0.000000000000000000 ) ) ;
#4654 = ADVANCED_FACE ( 'NONE', ( #629 ), #5590, .T. ) ;
#4655 = DIRECTION ( 'NONE',  ( -0.000000000000000000, -1.000000000000000000, -0.000000000000000000 ) ) ;
#4656 = ADVANCED_FACE ( 'NONE', ( #10855 ), #8800, .F. ) ;
#4657 = DIRECTION ( 'NONE',  ( 0.000000000000000000, 0.000000000000000000, 1.000000000000000000 ) ) ;
#4658 = CARTESIAN_POINT ( 'NONE',  ( -24.35964822603314772, 52.63541666571061484, -4.064049460664953983 ) ) ;
#4659 = CARTESIAN_POINT ( 'NONE',  ( 24.49999999999999289, -6.767949192431104599, 10.00000000000001243 ) ) ;
#4660 = CARTESIAN_POINT ( 'NONE',  ( -27.98076211353308196, 55.47306177707831409, -4.543495204426306167 ) ) ;
#4661 = ORIENTED_EDGE ( 'NONE', *, *, #2943, .T. ) ;
#4662 = CONICAL_SURFACE ( 'NONE', #36, 1.615000000000000213, 0.9599310885968811435 ) ;
#4663 = DIRECTION ( 'NONE',  ( 0.000000000000000000, 0.000000000000000000, 1.000000000000000000 ) ) ;
#4664 = CONTEXT_DEPENDENT_SHAPE_REPRESENTATION ( #4227, #3783 ) ;
#4665 = VERTEX_POINT ( 'NONE', #5857 ) ;
#4666 = CARTESIAN_POINT ( 'NONE',  ( -27.78269821382355431, 55.90794815475196344, -4.132229125461595487 ) ) ;
#4667 = EDGE_CURVE ( 'NONE', #783, #8160, #10283, .T. ) ;
#4668 = CARTESIAN_POINT ( 'NONE',  ( -25.17020516978313083, 49.83541666571061768, -6.403925809002825709 ) ) ;
#4669 = VECTOR ( 'NONE', #8200, 1000.000000000000000 ) ;
#4670 = CARTESIAN_POINT ( 'NONE',  ( 19.01572293645009637, 17.10672457250295508, 11.01141524516921422 ) ) ;
#4671 = ORIENTED_EDGE ( 'NONE', *, *, #6135, .T. ) ;
#4672 = EDGE_CURVE ( 'NONE', #5073, #9475, #8103, .T. ) ;
#4673 = CARTESIAN_POINT ( 'NONE',  ( -26.79131905728310059, 55.26041666571061484, -3.596074190997381237 ) ) ;
#4674 = ORIENTED_EDGE ( 'NONE', *, *, #623, .T. ) ;
#4675 = DIRECTION ( 'NONE',  ( 1.000000000000000000, 0.000000000000000000, 0.000000000000000000 ) ) ;
#4676 = ORIENTED_EDGE ( 'NONE', *, *, #7169, .T. ) ;
#4677 = CARTESIAN_POINT ( 'NONE',  ( 1.720978244806805169, 31.81455566112594013, 12.50219158473306358 ) ) ;
#4678 = B_SPLINE_CURVE_WITH_KNOTS ( 'NONE', 3,
 ( #5285, #3508, #8503, #166, #4284, #7674 ),
 .UNSPECIFIED., .F., .F.,
 ( 4, 2, 4 ),
 ( 0.002365888236228001588, 0.003551327329835089319, 0.004736766423442177049 ),
 .UNSPECIFIED. ) ;
#4679 = SURFACE_STYLE_USAGE ( .BOTH. , #2125 ) ;
#4680 = ORIENTED_EDGE ( 'NONE', *, *, #5270, .T. ) ;
#4681 = CARTESIAN_POINT ( 'NONE',  ( 22.83430298279833437, 18.47273307877622983, 10.95195840513859231 ) ) ;
#4682 =( NAMED_UNIT ( * ) SI_UNIT ( $, .STERADIAN. ) SOLID_ANGLE_UNIT ( ) );
#4683 = EDGE_CURVE ( 'NONE', #4873, #2508, #10085, .T. ) ;
#4684 = DIRECTION ( 'NONE',  ( 0.000000000000000000, 0.000000000000000000, -1.000000000000000000 ) ) ;
#4685 = CARTESIAN_POINT ( 'NONE',  ( 18.31593954903570776, 16.96748919427588831, 13.03503021400358541 ) ) ;
#4686 = DIRECTION ( 'NONE',  ( -1.000000000000000000, -0.000000000000000000, -0.000000000000000000 ) ) ;
#4687 = DIRECTION ( 'NONE',  ( 0.000000000000000000, 0.000000000000000000, -1.000000000000000000 ) ) ;
#4688 = DIRECTION ( 'NONE',  ( 0.000000000000000000, 0.000000000000000000, 1.000000000000000000 ) ) ;
#4689 = EDGE_LOOP ( 'NONE', ( #8781, #2810, #3046, #8292, #729 ) ) ;
#4690 = ORIENTED_EDGE ( 'NONE', *, *, #441, .F. ) ;
#4691 = CARTESIAN_POINT ( 'NONE',  ( 17.17871587691444546, 17.77103159139232957, 13.12322671172946897 ) ) ;
#4692 = ADVANCED_FACE ( 'NONE', ( #1692 ), #1695, .F. ) ;
#4693 = AXIS2_PLACEMENT_3D ( 'NONE', #10213, #10107, #3497 ) ;
#4694 = DIRECTION ( 'NONE',  ( -1.000000000000000000, -0.000000000000000000, -0.000000000000000000 ) ) ;
#4695 = CARTESIAN_POINT ( 'NONE',  ( 0.000000000000000000, 3.031088913245550742, 1.749999999999972466 ) ) ;
#4696 = FACE_OUTER_BOUND ( 'NONE', #5927, .T. ) ;
#4697 = CARTESIAN_POINT ( 'NONE',  ( -24.98076211353213694, 57.86529025992057029, -6.732050807568382922 ) ) ;
#4698 =( NAMED_UNIT ( * ) SI_UNIT ( $, .STERADIAN. ) SOLID_ANGLE_UNIT ( ) );
#4699 = CARTESIAN_POINT ( 'NONE',  ( -1.449747468305836229, 33.50000000000000000, 16.23437500000000355 ) ) ;
#4700 = CARTESIAN_POINT ( 'NONE',  ( 34.99999999999999289, 1.000000000000004663, -11.50000000000000533 ) ) ;
#4701 = AXIS2_PLACEMENT_3D ( 'NONE', #1604, #10271, #5990 ) ;
#4702 = ORIENTED_EDGE ( 'NONE', *, *, #7653, .F. ) ;
#4703 = CARTESIAN_POINT ( 'NONE',  ( 27.50000000000000711, 0.5000000000000162093, 10.00000000000000888 ) ) ;
#4704 = CARTESIAN_POINT ( 'NONE',  ( 2.472591809326055046, 28.89829686842209355, 16.76343341526694175 ) ) ;
#4705 = AXIS2_PLACEMENT_3D ( 'NONE', #2919, #1975, #9630 ) ;
#4706 = CARTESIAN_POINT ( 'NONE',  ( 0.000000000000000000, 0.000000000000000000, -0.3080913168122742518 ) ) ;
#4707 = EDGE_CURVE ( 'NONE', #10104, #7106, #3477, .T. ) ;
#4708 = CLOSED_SHELL ( 'NONE', ( #7780, #2015, #1321, #7507, #7568, #10629, #938, #2360, #8977, #5899, #8024, #4887, #1725, #2706, #2331, #4460, #4692, #2688, #8845, #87 ) ) ;
#4709 = DIRECTION ( 'NONE',  ( -1.000000000000000000, -0.000000000000000000, -0.000000000000000000 ) ) ;
#4710 = FACE_OUTER_BOUND ( 'NONE', #10933, .T. ) ;
#4711 = CARTESIAN_POINT ( 'NONE',  ( -27.98076211353308551, 51.30833333333320212, -3.845299461620869330 ) ) ;
#4712 = CARTESIAN_POINT ( 'NONE',  ( -27.60187600103308014, 51.58541666571061768, -5.935950539335252074 ) ) ;
#4713 = CARTESIAN_POINT ( 'NONE',  ( 3.200000000000000178, -2.020725942163647648, 3.499999999999999556 ) ) ;
#4714 = CARTESIAN_POINT ( 'NONE',  ( -2.742827927723112236, -3.035229711105190464, -3.433252694550595230 ) ) ;
#4715 = CONICAL_SURFACE ( 'NONE', #5069, 2.500000000000000888, 0.9599310885968785900 ) ;
#4716 = ORIENTED_EDGE ( 'NONE', *, *, #6266, .T. ) ;
#4717 = CIRCLE ( 'NONE', #8963, 2.767949192431121919 ) ;
#4718 = DIRECTION ( 'NONE',  ( 1.000000000000000000, -0.000000000000000000, 1.156482317317871478E-16 ) ) ;
#4719 = AXIS2_PLACEMENT_3D ( 'NONE', #7409, #2355, #4021 ) ;
#4720 = CARTESIAN_POINT ( 'NONE',  ( 2.500000000000000000, 1.178949249685213863, -2.042000000000001148 ) ) ;
#4721 = ADVANCED_FACE ( 'NONE', ( #907 ), #4132, .T. ) ;
#4722 = APPLICATION_PROTOCOL_DEFINITION ( 'draft international standard', 'automotive_design', 1998, #7209 ) ;
#4723 = ORIENTED_EDGE ( 'NONE', *, *, #4324, .F. ) ;
#4724 = ADVANCED_FACE ( 'NONE', ( #2589 ), #854, .F. ) ;
#4725 = DIRECTION ( 'NONE',  ( 0.000000000000000000, 0.000000000000000000, 1.000000000000000000 ) ) ;
#4726 = CIRCLE ( 'NONE', #9501, 3.500000000000591971 ) ;
#4727 = CARTESIAN_POINT ( 'NONE',  ( -24.35964822603314772, 51.17708333237728624, -5.935950539335252074 ) ) ;
#4728 = CARTESIAN_POINT ( 'NONE',  ( 20.44553565182888732, 18.02736169756263962, 11.00732503135576401 ) ) ;
#4729 = VERTEX_POINT ( 'NONE', #7754 ) ;
#4730 = CARTESIAN_POINT ( 'NONE',  ( -25.98076211353311393, 54.96874999904394343, -6.871901078670400231 ) ) ;
#4731 = EDGE_CURVE ( 'NONE', #4732, #6644, #9, .T. ) ;
#4732 = VERTEX_POINT ( 'NONE', #4256 ) ;
#4733 = DIRECTION ( 'NONE',  ( 0.000000000000000000, 1.000000000000000000, 0.000000000000000000 ) ) ;
#4734 = ORIENTED_EDGE ( 'NONE', *, *, #10918, .F. ) ;
#4735 = CARTESIAN_POINT ( 'NONE',  ( -2.500000000000005773, 29.99999999999999645, 15.21875000000000355 ) ) ;
#4736 = SURFACE_STYLE_FILL_AREA ( #5564 ) ;
#4737 = CIRCLE ( 'NONE', #5779, 4.999999999999997335 ) ;
#4738 = VERTEX_POINT ( 'NONE', #10024 ) ;
#4739 = CARTESIAN_POINT ( 'NONE',  ( 15.98809489411982199, 17.54743901181251786, 11.16417930307855677 ) ) ;
#4740 = SURFACE_SIDE_STYLE ('',( #6337 ) ) ;
#4741 = EDGE_CURVE ( 'NONE', #8576, #990, #4470, .T. ) ;
#4742 = ADVANCED_FACE ( 'NONE', ( #5199 ), #8612, .T. ) ;
#4743 = CARTESIAN_POINT ( 'NONE',  ( 4.211140560182196957, 2.431303136016536470, -3.745885042887433514 ) ) ;
#4744 = CARTESIAN_POINT ( 'NONE',  ( 22.47009348518006888, 19.30075366110858326, 13.00425721518280042 ) ) ;
#4745 = VECTOR ( 'NONE', #4863, 1000.000000000000000 ) ;
#4746 = CARTESIAN_POINT ( 'NONE',  ( -23.98076211353314235, 52.27083333142136468, -6.154700538379337615 ) ) ;
#4747 = CARTESIAN_POINT ( 'NONE',  ( -26.51666049839535688, 53.20626073911682141, -7.000000000000071942 ) ) ;
#4748 = DIRECTION ( 'NONE',  ( 0.000000000000000000, 1.000000000000000000, -1.345283343056720273E-15 ) ) ;
#4749 = EDGE_LOOP ( 'NONE', ( #1505, #6420, #5452, #699 ) ) ;
#4750 = ORIENTED_EDGE ( 'NONE', *, *, #10041, .F. ) ;
#4751 = CARTESIAN_POINT ( 'NONE',  ( 17.50063742165245984, 17.44909550871243198, 13.09303515564029397 ) ) ;
#4752 = DIRECTION ( 'NONE',  ( -0.000000000000000000, 1.000000000000000000, -0.000000000000000000 ) ) ;
#4753 =( BOUNDED_CURVE ( )  B_SPLINE_CURVE ( 2, ( #399, #7974, #2024, #3799, #8076, #9022, #1411 ),
 .UNSPECIFIED., .F., .F. ) 
 B_SPLINE_CURVE_WITH_KNOTS ( ( 3, 2, 2, 3 ),
 ( 0.9166666666666666297, 0.9259259259259259300, 0.9444444444444444198, 0.9524107084371162824 ),
 .UNSPECIFIED. ) 
 CURVE ( )  GEOMETRIC_REPRESENTATION_ITEM ( )  RATIONAL_B_SPLINE_CURVE ( ( 0.9330127018922194093, 0.9330127018922189652, 1.000000000000000000, 0.8660254037844387076, 1.000000000000000000, 0.9423670419047019964, 0.9343189745669037150 ) ) 
 REPRESENTATION_ITEM ( '' )  );
#4754 = AXIS2_PLACEMENT_3D ( 'NONE', #462, #4599, #1135 ) ;
#4755 = DIRECTION ( 'NONE',  ( -0.000000000000000000, -0.000000000000000000, 1.000000000000000000 ) ) ;
#4756 = CARTESIAN_POINT ( 'NONE',  ( 2.500000000000000000, 2.357898499370433054, -1.951563910473907981E-15 ) ) ;
#4757 = EDGE_CURVE ( 'NONE', #9093, #281, #10387, .T. ) ;
#4758 = CARTESIAN_POINT ( 'NONE',  ( -3.527408190673960053, 31.38357824266065066, 14.14281658473306713 ) ) ;
#4759 = CARTESIAN_POINT ( 'NONE',  ( 3.200000000000000178, -2.020725942163728028, -3.499999999999999556 ) ) ;
#4760 = ORIENTED_EDGE ( 'NONE', *, *, #9317, .T. ) ;
#4761 = DIRECTION ( 'NONE',  ( 0.000000000000000000, 0.000000000000000000, 1.000000000000000000 ) ) ;
#4762 = CIRCLE ( 'NONE', #8841, 2.499999999999999556 ) ;
#4763 = VECTOR ( 'NONE', #3641, 1000.000000000000000 ) ;
#4764 = CARTESIAN_POINT ( 'NONE',  ( -2.428085025993355295, 32.52166244231248271, 16.06030841526693820 ) ) ;
#4765 = CARTESIAN_POINT ( 'NONE',  ( -4.000000000000000000, 1.677772373332757194, -3.535253723897187506 ) ) ;
#4766 = CARTESIAN_POINT ( 'NONE',  ( 5.076455387921338769, 24.47916666666667140, 0.000000000000000000 ) ) ;
#4767 = CARTESIAN_POINT ( 'NONE',  ( 2.500000000000000000, -1.768423874527823569, 1.021000000000002794 ) ) ;
#4768 = DIRECTION ( 'NONE',  ( -1.000000000000000000, -0.000000000000000000, -0.000000000000000000 ) ) ;
#4769 = CARTESIAN_POINT ( 'NONE',  ( -27.60187600103308014, 50.88541666571062194, -5.935950539335252074 ) ) ;
#4770 = LINE ( 'NONE', #6627, #3419 ) ;
#4771 = COLOUR_RGB ( '', 0.08235294, 0.09019608, 0.10196078) ;
#4772 = DIRECTION ( 'NONE',  ( -1.000000000000000000, -0.000000000000000000, -0.000000000000000000 ) ) ;
#4773 = VERTEX_POINT ( 'NONE', #9187 ) ;
#4774 = CARTESIAN_POINT ( 'NONE',  ( -25.44486372867087454, 54.16876073720499818, -3.000000000000134559 ) ) ;
#4775 = FACE_OUTER_BOUND ( 'NONE', #1918, .T. ) ;
#4776 = CONTEXT_DEPENDENT_SHAPE_REPRESENTATION ( #9463, #396 ) ;
#4777 = VERTEX_POINT ( 'NONE', #1580 ) ;
#4778 = CARTESIAN_POINT ( 'NONE',  ( 0.3126073911691312213, -2.020725942164384836, 3.499999999999999556 ) ) ;
#4779 = CARTESIAN_POINT ( 'NONE',  ( 2.000000000000000444, 3.464101615137754830, -3.142992957459231018 ) ) ;
#4780 = PRODUCT_RELATED_PRODUCT_CATEGORY ( 'part', '', ( #218 ) ) ;
#4781 = CARTESIAN_POINT ( 'NONE',  ( 19.91130943667480224, 20.32997460694367575, 11.00732503135576401 ) ) ;
#4782 = EDGE_LOOP ( 'NONE', ( #3186, #7899, #8361, #5934 ) ) ;
#4783 = FACE_OUTER_BOUND ( 'NONE', #9355, .T. ) ;
#4784 = EDGE_LOOP ( 'NONE', ( #6994, #5194 ) ) ;
#4785 = DIRECTION ( 'NONE',  ( 0.7512361908166128588, 0.6577071706380231975, 0.05536662621716938876 ) ) ;
#4786 = ORIENTED_EDGE ( 'NONE', *, *, #2003, .T. ) ;
#4787 = DIRECTION ( 'NONE',  ( 0.000000000000000000, -1.000000000000000000, 1.287488025362403787E-15 ) ) ;
#4788 =( LENGTH_UNIT ( ) NAMED_UNIT ( * ) SI_UNIT ( .MILLI., .METRE. ) );
#4789 = ORIENTED_EDGE ( 'NONE', *, *, #9452, .T. ) ;
#4790 = CARTESIAN_POINT ( 'NONE',  ( 16.61199375056689931, 16.92354015536430722, 11.10566822806672427 ) ) ;
#4791 = SHAPE_REPRESENTATION_RELATIONSHIP ( 'NONE' , 'NONE' ,  #1223, #6261 ) ;
#4792 = ADVANCED_FACE ( 'NONE', ( #7971 ), #5254, .T. ) ;
#4793 = CARTESIAN_POINT ( 'NONE',  ( 4.000000000000001776, 0.000000000000000000, -2.200000000000001066 ) ) ;
#4794 = EDGE_CURVE ( 'NONE', #3414, #4665, #9356, .T. ) ;
#4795 = CARTESIAN_POINT ( 'NONE',  ( 22.89753608554585540, 18.38182967998604056, 12.94889058896590583 ) ) ;
#4796 = CARTESIAN_POINT ( 'NONE',  ( -25.98076211353311393, 52.73749999808804034, -2.690598923241634743 ) ) ;
#4797 = DIRECTION ( 'NONE',  ( 0.000000000000000000, 0.000000000000000000, -1.000000000000000000 ) ) ;
#4798 = DIRECTION ( 'NONE',  ( -1.000000000000000000, -0.000000000000000000, -0.000000000000000000 ) ) ;
#4799 = ORIENTED_EDGE ( 'NONE', *, *, #10746, .F. ) ;
#4800 = ORIENTED_EDGE ( 'NONE', *, *, #4342, .F. ) ;
#4801 = CARTESIAN_POINT ( 'NONE',  ( 19.32345233471135515, 17.12110500680467240, 13.00476395487764947 ) ) ;
#4802 = B_SPLINE_CURVE_WITH_KNOTS ( 'NONE', 3,
 ( #8481, #864, #8539, #7533 ),
 .UNSPECIFIED., .F., .F.,
 ( 4, 4 ),
 ( 0.000000000000000000, 0.002452478801916376308 ),
 .UNSPECIFIED. ) ;
#4803 = CARTESIAN_POINT ( 'NONE',  ( 3.200000000000000178, 4.041451884327400101, -2.303506639521620593E-14 ) ) ;
#4804 = DIRECTION ( 'NONE',  ( 0.000000000000000000, -0.000000000000000000, -1.000000000000000000 ) ) ;
#4805 = DIRECTION ( 'NONE',  ( 0.000000000000000000, 0.000000000000000000, 1.000000000000000000 ) ) ;
#4806 = FACE_OUTER_BOUND ( 'NONE', #5220, .T. ) ;
#4807 = CARTESIAN_POINT ( 'NONE',  ( -2.527408190673963162, 30.96936468028755840, 12.89281658473306535 ) ) ;
#4808 = DIRECTION ( 'NONE',  ( 1.000000000000000000, 0.000000000000000000, 0.000000000000000000 ) ) ;
#4809 = EDGE_LOOP ( 'NONE', ( #9316, #9508, #850, #3113, #278, #2721 ) ) ;
#4810 = CARTESIAN_POINT ( 'NONE',  ( 21.55579831881754416, 20.86490736922957367, 2.500000000000000444 ) ) ;
#4811 = VERTEX_POINT ( 'NONE', #1125 ) ;
#4812 = CARTESIAN_POINT ( 'NONE',  ( -1.814555661125937247, 28.27902175519318817, 16.37280841526694175 ) ) ;
#4813 = FACE_OUTER_BOUND ( 'NONE', #3281, .T. ) ;
#4814 = CARTESIAN_POINT ( 'NONE',  ( 17.13192716875488131, 17.81782029955189728, 12.12541829646253078 ) ) ;
#4815 = DIRECTION ( 'NONE',  ( -1.000000000000000000, -0.000000000000000000, -0.000000000000000000 ) ) ;
#4816 = ADVANCED_BREP_SHAPE_REPRESENTATION ( '', ( #1777, #308 ), #8995 ) ;
#4817 = CARTESIAN_POINT ( 'NONE',  ( -2.725741868435985094, 3.045094352034055429, -3.220599429844047012 ) ) ;
#4818 = CARTESIAN_POINT ( 'NONE',  ( -25.17020516978313083, 51.70208333237728482, -3.596074190997380349 ) ) ;
#4819 = EDGE_CURVE ( 'NONE', #9208, #874, #5309, .T. ) ;
#4820 = PLANE ( 'NONE',  #9622 ) ;
#4821 = DIRECTION ( 'NONE',  ( 0.000000000000000000, -0.5000000000000011102, -0.8660254037844379305 ) ) ;
#4822 = AXIS2_PLACEMENT_3D ( 'NONE', #2704, #1022, #3589 ) ;
#4823 = EDGE_LOOP ( 'NONE', ( #8127, #3242 ) ) ;
#4824 = CARTESIAN_POINT ( 'NONE',  ( -2.474873734152916338, 27.52512626584707789, 14.12500000000000355 ) ) ;
#4825 = CYLINDRICAL_SURFACE ( 'NONE', #7889, 2.000000000000000888 ) ;
#4826 = ITEM_DEFINED_TRANSFORMATION ( 'NONE', 'NONE', #2620,  #308 ) ;
#4827 = DIRECTION ( 'NONE',  ( 1.000000000000000000, 0.000000000000000000, -0.000000000000000000 ) ) ;
#4828 = CIRCLE ( 'NONE', #8900, 5.560781378645573980 ) ;
#4829 = CARTESIAN_POINT ( 'NONE',  ( -24.35964822603314417, 53.21874999904395764, -5.000000000000103029 ) ) ;
#4830 = CARTESIAN_POINT ( 'NONE',  ( 17.86810043078960319, 17.16701444005803268, 12.06109941161078325 ) ) ;
#4831 = CARTESIAN_POINT ( 'NONE',  ( -25.17020516978313083, 55.43541666571061910, -6.403925809002825709 ) ) ;
#4832 = ORIENTED_EDGE ( 'NONE', *, *, #372, .F. ) ;
#4833 = CARTESIAN_POINT ( 'NONE',  ( -27.60187600103308725, 55.86681146796335895, -4.629981812462977686 ) ) ;
#4834 = EDGE_LOOP ( 'NONE', ( #5881, #4919, #5560, #1551, #3071, #8100 ) ) ;
#4835 = CARTESIAN_POINT ( 'NONE',  ( 29.49999999999999645, -3.999999999999993339, -7.149999999999983480 ) ) ;
#4836 = ORIENTED_EDGE ( 'NONE', *, *, #5735, .T. ) ;
#4837 = DIRECTION ( 'NONE',  ( 1.000000000000000000, 0.000000000000000000, 0.000000000000000000 ) ) ;
#4838 = ORIENTED_EDGE ( 'NONE', *, *, #10968, .T. ) ;
#4839 = CARTESIAN_POINT ( 'NONE',  ( 20.70533613433985920, 18.20808090964021986, 11.00732503135576401 ) ) ;
#4840 = VECTOR ( 'NONE', #3378, 1000.000000000000000 ) ;
#4841 = EDGE_CURVE ( 'NONE', #10063, #8739, #3313, .T. ) ;
#4842 = CARTESIAN_POINT ( 'NONE',  ( -0.1750025118121544265, -4.719839900820635314, -3.469254087858253399 ) ) ;
#4843 = CARTESIAN_POINT ( 'NONE',  ( 18.68606934758710025, 15.93178998805769453, 12.97541080761745924 ) ) ;
#4844 = CARTESIAN_POINT ( 'NONE',  ( -23.98076211353314235, 50.17083333142137036, -6.154700538379337615 ) ) ;
#4845 = CARTESIAN_POINT ( 'NONE',  ( 34.93373351399774407, 2.154066368359273564, -4.530732988813361395 ) ) ;
#4846 = LINE ( 'NONE', #9845, #10608 ) ;
#4847 = VERTEX_POINT ( 'NONE', #5471 ) ;
#4848 = CARTESIAN_POINT ( 'NONE',  ( -2.428085025993355295, 32.52166244231248271, 16.06030841526693820 ) ) ;
#4849 = VERTEX_POINT ( 'NONE', #8695 ) ;
#4850 = EDGE_CURVE ( 'NONE', #101, #10992, #3689, .T. ) ;
#4851 = CARTESIAN_POINT ( 'NONE',  ( 19.98916778955327800, 17.57501987461890991, 13.00425721518307576 ) ) ;
#4852 = ADVANCED_FACE ( 'NONE', ( #9688 ), #7813, .T. ) ;
#4853 = CARTESIAN_POINT ( 'NONE',  ( -25.98076211353311393, 49.49999999999986500, -3.000000000000131894 ) ) ;
#4854 = DIRECTION ( 'NONE',  ( 1.000000000000000000, 0.000000000000000000, 0.000000000000000000 ) ) ;
#4855 = DIRECTION ( 'NONE',  ( -1.000000000000000000, -0.000000000000000000, -0.000000000000000000 ) ) ;
#4856 = CARTESIAN_POINT ( 'NONE',  ( 2.472591809326049272, 31.10170313157791711, 13.67406658473306535 ) ) ;
#4857 = CARTESIAN_POINT ( 'NONE',  ( 2.000000000000000000, 1.329782007511006281, 0.7677499999999984892 ) ) ;
#4858 = ORIENTED_EDGE ( 'NONE', *, *, #3519, .F. ) ;
#4859 = CARTESIAN_POINT ( 'NONE',  ( 4.800000000000000711, 0.000000000000000000, 0.000000000000000000 ) ) ;
#4860 = EDGE_CURVE ( 'NONE', #947, #6804, #6122, .T. ) ;
#4861 = VERTEX_POINT ( 'NONE', #1183 ) ;
#4862 = CARTESIAN_POINT ( 'NONE',  ( 1.101703131577913553, 32.47259180932605460, 17.07593341526694530 ) ) ;
#4863 = DIRECTION ( 'NONE',  ( 1.000000000000000000, 6.098637220230963674E-17, 0.000000000000000000 ) ) ;
#4864 = DIRECTION ( 'NONE',  ( 1.000000000000000000, -0.000000000000000000, 1.156482317317871478E-16 ) ) ;
#4865 = CARTESIAN_POINT ( 'NONE',  ( -23.98076211353314235, 50.11249999808803324, -5.000000000000103029 ) ) ;
#4866 = ADVANCED_FACE ( 'NONE', ( #3742, #2865 ), #295, .T. ) ;
#4867 = ADVANCED_FACE ( 'NONE', ( #9628 ), #2021, .F. ) ;
#4868 = CARTESIAN_POINT ( 'NONE',  ( 34.91780110604603493, 2.399866884679865198, 3.990594396599065341 ) ) ;
#4869 = CARTESIAN_POINT ( 'NONE',  ( -26.79131905728310059, 55.02708333237728056, -6.403925809002825709 ) ) ;
#4870 = AXIS2_PLACEMENT_3D ( 'NONE', #8663, #2781, #10442 ) ;
#4871 = DIRECTION ( 'NONE',  ( 0.000000000000000000, 0.000000000000000000, 1.000000000000000000 ) ) ;
#4872 = CARTESIAN_POINT ( 'NONE',  ( 4.000000000000000000, 2.512223110932545023, -3.469391141908803711 ) ) ;
#4873 = VERTEX_POINT ( 'NONE', #6076 ) ;
#4874 = LINE ( 'NONE', #7368, #4669 ) ;
#4875 = MECHANICAL_DESIGN_GEOMETRIC_PRESENTATION_REPRESENTATION (  '', ( #3271 ), #72 ) ;
#4876 = DIRECTION ( 'NONE',  ( 1.000000000000000000, 0.000000000000000000, 0.000000000000000000 ) ) ;
#4877 = AXIS2_PLACEMENT_3D ( 'NONE', #3162, #9002, #10715 ) ;
#4878 = DIRECTION ( 'NONE',  ( -1.000000000000000000, -0.000000000000000000, -0.000000000000000000 ) ) ;
#4879 = CARTESIAN_POINT ( 'NONE',  ( -25.98076211353310683, 51.99374999904394912, -6.871901078670399343 ) ) ;
#4880 = VECTOR ( 'NONE', #7097, 1000.000000000000114 ) ;
#4881 = CARTESIAN_POINT ( 'NONE',  ( 23.11946528304491011, 21.60344811844516499, 11.00732503135595941 ) ) ;
#4882 = CARTESIAN_POINT ( 'NONE',  ( -25.98076211353311393, 50.37499999999986500, -7.309401076758571314 ) ) ;
#4883 = VECTOR ( 'NONE', #9270, 1000.000000000000114 ) ;
#4884 = VERTEX_POINT ( 'NONE', #10306 ) ;
#4885 = DIRECTION ( 'NONE',  ( 0.000000000000000000, -1.224646799147353207E-16, 1.000000000000000000 ) ) ;
#4886 = ADVANCED_FACE ( 'NONE', ( #2701 ), #9466, .T. ) ;
#4887 = ADVANCED_FACE ( 'NONE', ( #8637, #7030, #4430 ), #6969, .F. ) ;
#4888 = ORIENTED_EDGE ( 'NONE', *, *, #372, .T. ) ;
#4889 = ORIENTED_EDGE ( 'NONE', *, *, #3510, .T. ) ;
#4890 = CARTESIAN_POINT ( 'NONE',  ( 3.200000000000000178, 4.127059713126577826E-16, 3.369999999999997886 ) ) ;
#4891 = VERTEX_POINT ( 'NONE', #7864 ) ;
#4892 = CARTESIAN_POINT ( 'NONE',  ( 3.199999999999999734, 0.000000000000000000, 0.000000000000000000 ) ) ;
#4893 = DIRECTION ( 'NONE',  ( 0.000000000000000000, 0.000000000000000000, 1.000000000000000000 ) ) ;
#4894 = VECTOR ( 'NONE', #1528, 1000.000000000000000 ) ;
#4895 = ORIENTED_EDGE ( 'NONE', *, *, #1713, .F. ) ;
#4896 = CARTESIAN_POINT ( 'NONE',  ( 19.52039169078502212, 17.38380627596665562, 11.00732402621840578 ) ) ;
#4897 = SURFACE_STYLE_USAGE ( .BOTH. , #10058 ) ;
#4898 = CIRCLE ( 'NONE', #1704, 3.249999999999998668 ) ;
#4899 = FACE_OUTER_BOUND ( 'NONE', #5052, .T. ) ;
#4900 = CARTESIAN_POINT ( 'NONE',  ( 2.807080416178989513, -3.225969019225150003, -3.502507215260505014 ) ) ;
#4901 = CARTESIAN_POINT ( 'NONE',  ( 23.68215991433358525, 19.03072201379386641, 12.94889058896590583 ) ) ;
#4902 = CIRCLE ( 'NONE', #2955, 2.100000000000000089 ) ;
#4903 = CARTESIAN_POINT ( 'NONE',  ( -24.98076211353312814, 52.32916666475470180, -6.732050807568954909 ) ) ;
#4904 = CIRCLE ( 'NONE', #9337, 3.249999999999998668 ) ;
#4905 = CARTESIAN_POINT ( 'NONE',  ( 34.64101615137754919, 5.000000000000002665, -2.500000000000000000 ) ) ;
#4906 = FACE_OUTER_BOUND ( 'NONE', #155, .T. ) ;
#4907 = PRODUCT_DEFINITION_CONTEXT ( 'detailed design', #10976, 'design' ) ;
#4908 = EDGE_CURVE ( 'NONE', #8322, #7216, #237, .T. ) ;
#4909 = ORIENTED_EDGE ( 'NONE', *, *, #740, .T. ) ;
#4910 = CARTESIAN_POINT ( 'NONE',  ( 3.527408190673964494, 31.38357824266065776, 16.91968341526693820 ) ) ;
#4911 = EDGE_LOOP ( 'NONE', ( #2521, #1441, #3072, #9986, #7950, #8373, #5951 ) ) ;
#4912 = CARTESIAN_POINT ( 'NONE',  ( 22.86397682584157565, 19.61629903322988966, 13.00425721518307753 ) ) ;
#4913 = CARTESIAN_POINT ( 'NONE',  ( 6.015568632492061418, 34.47916666666664298, 2.500000000000000000 ) ) ;
#4914 = DIRECTION ( 'NONE',  ( 0.000000000000000000, -0.000000000000000000, -1.000000000000000000 ) ) ;
#4915 = CARTESIAN_POINT ( 'NONE',  ( 29.17190429162964094, 2.000000000000001776, 2.500000000000000000 ) ) ;
#4916 = CARTESIAN_POINT ( 'NONE',  ( -1.515916693951010252, 33.47259180932604750, 13.98656658473306713 ) ) ;
#4917 = EDGE_CURVE ( 'NONE', #10021, #6926, #2812, .T. ) ;
#4918 = DIRECTION ( 'NONE',  ( -0.000000000000000000, -0.000000000000000000, 1.000000000000000000 ) ) ;
#4919 = ORIENTED_EDGE ( 'NONE', *, *, #1594, .T. ) ;
#4920 = CARTESIAN_POINT ( 'NONE',  ( -25.98076211353324894, 14.99999999999984190, 2.500000000000000000 ) ) ;
#4921 = EDGE_CURVE ( 'NONE', #5409, #9236, #9520, .T. ) ;
#4922 = ORIENTED_EDGE ( 'NONE', *, *, #1796, .T. ) ;
#4923 = CARTESIAN_POINT ( 'NONE',  ( 0.3126073911696503060, 4.041451884327400101, -2.290628625700182053E-14 ) ) ;
#4924 = CARTESIAN_POINT ( 'NONE',  ( -4.000000000000000000, 2.511478553582031203, -3.469254451724764543 ) ) ;
#4925 =( BOUNDED_SURFACE ( )  B_SPLINE_SURFACE ( 3, 2, ( 
 ( #4493, #6308, #5321, #3704, #6198, #7093, #197, #4603, #5266, #10484, #2876, #6248, #1985, #5371, #5428, #148, #1032, #9642, #3595, #4442, #6929, #10318, #1198, #4381, #8705, #7985, #2713, #3757, #6982, #7876, #10537, #9701, #2932, #7768, #10369, #2097, #2768, #6144, #250, #7043, #10431 ),
 ( #3187, #6514, #10647, #4020, #3085, #9074, #8034, #8918, #3808, #9918, #464, #3916, #10692, #9029, #7300, #6458, #2304, #9863, #5695, #9807, #2252, #5647, #8191, #1420, #4812, #5744, #1470, #1308, #2193, #4704, #7250, #2990, #9757, #4862, #10741, #4651, #3867, #8974, #6568, #5588, #567 ),
 ( #8088, #8239, #2149, #3964, #7352, #3134, #627, #7408, #10801, #407, #6369, #9968, #3036, #5538, #7198, #10594, #2354, #1258, #6411, #1365, #4764, #8142, #518, #8915, #7927, #300, #402, #10532, #6243, #3802, #10643, #2926, #5583, #9637, #5532, #1304, #4538, #1077, #1979, #4487, #4644 ),
 ( #8869, #7088, #7036, #5366, #1252, #2188, #5481, #10588, #10479, #8029, #6193, #6299, #3859, #9751, #2821, #2028, #7871, #10423, #5422, #2091, #9695, #7136, #2142, #3697, #7192, #2870, #2984, #8810, #1190, #6363, #6405, #9580, #8749, #244, #1131, #4699, #8081, #458, #3642, #7244, #4595 ),
 ( #9802, #7979, #3750, #3031, #351, #4015, #677, #1360, #2467, #6678, #3912, #8968, #9857, #2347, #4074, #3238, #10076, #8345, #2299, #4916, #5790, #4758, #2246, #619, #10015, #3957, #7402, #7458, #8136, #513, #7292, #5739, #10686, #5690, #10795, #2404, #7345, #3297, #9119, #9068, #1414 ),
 ( #1515, #3078, #9177, #5640, #9913, #4807, #10735, #6452, #9024, #6611, #10847, #8185, #561, #1465, #10901, #4856, #8290, #3182, #1573, #3129, #4972, #6508, #725, #4125, #7513, #6563, #9963, #8230, #1630, #7573, #9403, #1683, #10963, #5027, #8399, #2693, #5850, #7, #63, #779, #5190 ),
 ( #4186, #845, #3469, #10349, #4247, #6018, #5083, #3354, #7632, #8572, #6735, #9232, #8521, #7806, #124, #3409, #8631, #7691, #6067, #10129, #2516, #5905, #3526, #8461, #898, #9288, #6789, #1850, #10184, #2579, #5245, #6850, #5961, #4422, #2643, #9349, #1746, #10298, #10243, #1009, #1801 ) ),
 .UNSPECIFIED., .T., .F., .F. ) 
 B_SPLINE_SURFACE_WITH_KNOTS ( ( 4, 3, 4 ),
 ( 3, 2, 2, 2, 2, 2, 2, 2, 2, 2, 2, 2, 2, 2, 2, 2, 2, 2, 2, 2, 3 ),
 ( 0.000000000000000000, 0.5000000000000000000, 1.000000000000000000 ),
 ( 0.000000000000000000, 0.04166666666666666435, 0.08333333333333332871, 0.1250000000000000000, 0.1666666666666666574, 0.2083333333333333426, 0.2500000000000000000, 0.2916666666666666852, 0.3333333333333333148, 0.3750000000000000000, 0.4166666666666666852, 0.4583333333333333148, 0.5000000000000000000, 0.5416666666666666297, 0.5833333333333333703, 0.6250000000000000000, 0.6666666666666666297, 0.7083333333333333703, 0.7500000000000000000, 0.7916666666666666297, 0.8001047462599640836 ),
 .UNSPECIFIED. ) 
 GEOMETRIC_REPRESENTATION_ITEM ( )  RATIONAL_B_SPLINE_SURFACE ( (
 ( 1.000000000000000000, 0.9238795325112867385, 1.000000000000000000, 0.9238795325112867385, 1.000000000000000000, 0.9238795325112867385, 1.000000000000000000, 0.9238795325112867385, 1.000000000000000000, 0.9238795325112867385, 1.000000000000000000, 0.9238795325112867385, 1.000000000000000000, 0.9238795325112867385, 1.000000000000000000, 0.9238795325112867385, 1.000000000000000000, 0.9238795325112867385, 1.000000000000000000, 0.9238795325112867385, 1.000000000000000000, 0.9238795325112867385, 1.000000000000000000, 0.9238795325112867385, 1.000000000000000000, 0.9238795325112867385, 1.000000000000000000, 0.9238795325112867385, 1.000000000000000000, 0.9238795325112867385, 1.000000000000000000, 0.9238795325112867385, 1.000000000000000000, 0.9238795325112867385, 1.000000000000000000, 0.9238795325112867385, 1.000000000000000000, 0.9238795325112867385, 1.000000000000000000, 0.9845845464796294522, 0.9754127805002987817),
 ( 0.3333333333333333703, 0.3079598441704289313, 0.3333333333333333703, 0.3079598441704289313, 0.3333333333333333703, 0.3079598441704289313, 0.3333333333333333703, 0.3079598441704289313, 0.3333333333333333703, 0.3079598441704289313, 0.3333333333333333703, 0.3079598441704289313, 0.3333333333333333703, 0.3079598441704289313, 0.3333333333333333703, 0.3079598441704289313, 0.3333333333333333703, 0.3079598441704289313, 0.3333333333333333703, 0.3079598441704289313, 0.3333333333333333703, 0.3079598441704289313, 0.3333333333333333703, 0.3079598441704289313, 0.3333333333333333703, 0.3079598441704289313, 0.3333333333333333703, 0.3079598441704289313, 0.3333333333333333703, 0.3079598441704289313, 0.3333333333333333703, 0.3079598441704289313, 0.3333333333333333703, 0.3079598441704289313, 0.3333333333333333703, 0.3079598441704289313, 0.3333333333333333703, 0.3079598441704289313, 0.3333333333333333703, 0.3281948488265432062, 0.3251375935000996309),
 ( 0.3333333333333333703, 0.3079598441704289313, 0.3333333333333333703, 0.3079598441704289313, 0.3333333333333333703, 0.3079598441704289313, 0.3333333333333333703, 0.3079598441704289313, 0.3333333333333333703, 0.3079598441704289313, 0.3333333333333333703, 0.3079598441704289313, 0.3333333333333333703, 0.3079598441704289313, 0.3333333333333333703, 0.3079598441704289313, 0.3333333333333333703, 0.3079598441704289313, 0.3333333333333333703, 0.3079598441704289313, 0.3333333333333333703, 0.3079598441704289313, 0.3333333333333333703, 0.3079598441704289313, 0.3333333333333333703, 0.3079598441704289313, 0.3333333333333333703, 0.3079598441704289313, 0.3333333333333333703, 0.3079598441704289313, 0.3333333333333333703, 0.3079598441704289313, 0.3333333333333333703, 0.3079598441704289313, 0.3333333333333333703, 0.3079598441704289313, 0.3333333333333333703, 0.3079598441704289313, 0.3333333333333333703, 0.3281948488265432062, 0.3251375935000996309),
 ( 1.000000000000000000, 0.9238795325112867385, 1.000000000000000000, 0.9238795325112867385, 1.000000000000000000, 0.9238795325112867385, 1.000000000000000000, 0.9238795325112867385, 1.000000000000000000, 0.9238795325112867385, 1.000000000000000000, 0.9238795325112867385, 1.000000000000000000, 0.9238795325112867385, 1.000000000000000000, 0.9238795325112867385, 1.000000000000000000, 0.9238795325112867385, 1.000000000000000000, 0.9238795325112867385, 1.000000000000000000, 0.9238795325112867385, 1.000000000000000000, 0.9238795325112867385, 1.000000000000000000, 0.9238795325112867385, 1.000000000000000000, 0.9238795325112867385, 1.000000000000000000, 0.9238795325112867385, 1.000000000000000000, 0.9238795325112867385, 1.000000000000000000, 0.9238795325112867385, 1.000000000000000000, 0.9238795325112867385, 1.000000000000000000, 0.9238795325112867385, 1.000000000000000000, 0.9845845464796294522, 0.9754127805002987817),
 ( 0.3333333333333333703, 0.3079598441704289313, 0.3333333333333333703, 0.3079598441704289313, 0.3333333333333333703, 0.3079598441704289313, 0.3333333333333333703, 0.3079598441704289313, 0.3333333333333333703, 0.3079598441704289313, 0.3333333333333333703, 0.3079598441704289313, 0.3333333333333333703, 0.3079598441704289313, 0.3333333333333333703, 0.3079598441704289313, 0.3333333333333333703, 0.3079598441704289313, 0.3333333333333333703, 0.3079598441704289313, 0.3333333333333333703, 0.3079598441704289313, 0.3333333333333333703, 0.3079598441704289313, 0.3333333333333333703, 0.3079598441704289313, 0.3333333333333333703, 0.3079598441704289313, 0.3333333333333333703, 0.3079598441704289313, 0.3333333333333333703, 0.3079598441704289313, 0.3333333333333333703, 0.3079598441704289313, 0.3333333333333333703, 0.3079598441704289313, 0.3333333333333333703, 0.3079598441704289313, 0.3333333333333333703, 0.3281948488265432062, 0.3251375935000996309),
 ( 0.3333333333333333703, 0.3079598441704289313, 0.3333333333333333703, 0.3079598441704289313, 0.3333333333333333703, 0.3079598441704289313, 0.3333333333333333703, 0.3079598441704289313, 0.3333333333333333703, 0.3079598441704289313, 0.3333333333333333703, 0.3079598441704289313, 0.3333333333333333703, 0.3079598441704289313, 0.3333333333333333703, 0.3079598441704289313, 0.3333333333333333703, 0.3079598441704289313, 0.3333333333333333703, 0.3079598441704289313, 0.3333333333333333703, 0.3079598441704289313, 0.3333333333333333703, 0.3079598441704289313, 0.3333333333333333703, 0.3079598441704289313, 0.3333333333333333703, 0.3079598441704289313, 0.3333333333333333703, 0.3079598441704289313, 0.3333333333333333703, 0.3079598441704289313, 0.3333333333333333703, 0.3079598441704289313, 0.3333333333333333703, 0.3079598441704289313, 0.3333333333333333703, 0.3079598441704289313, 0.3333333333333333703, 0.3281948488265432062, 0.3251375935000996309),
 ( 1.000000000000000000, 0.9238795325112867385, 1.000000000000000000, 0.9238795325112867385, 1.000000000000000000, 0.9238795325112867385, 1.000000000000000000, 0.9238795325112867385, 1.000000000000000000, 0.9238795325112867385, 1.000000000000000000, 0.9238795325112867385, 1.000000000000000000, 0.9238795325112867385, 1.000000000000000000, 0.9238795325112867385, 1.000000000000000000, 0.9238795325112867385, 1.000000000000000000, 0.9238795325112867385, 1.000000000000000000, 0.9238795325112867385, 1.000000000000000000, 0.9238795325112867385, 1.000000000000000000, 0.9238795325112867385, 1.000000000000000000, 0.9238795325112867385, 1.000000000000000000, 0.9238795325112867385, 1.000000000000000000, 0.9238795325112867385, 1.000000000000000000, 0.9238795325112867385, 1.000000000000000000, 0.9238795325112867385, 1.000000000000000000, 0.9238795325112867385, 1.000000000000000000, 0.9845845464796294522, 0.9754127805002987817) ) ) 
 REPRESENTATION_ITEM ( '' )  SURFACE ( )  );
#4926 = LINE ( 'NONE', #8091, #2036 ) ;
#4927 = DIRECTION ( 'NONE',  ( -1.000000000000000000, -0.000000000000000000, -0.000000000000000000 ) ) ;
#4928 = EDGE_CURVE ( 'NONE', #10824, #1334, #3797, .T. ) ;
#4929 = CARTESIAN_POINT ( 'NONE',  ( -25.98076211353311749, 56.99999999999884182, -7.000000000000094147 ) ) ;
#4930 = EDGE_CURVE ( 'NONE', #3329, #6272, #1341, .T. ) ;
#4931 = CARTESIAN_POINT ( 'NONE',  ( -27.60187600103308370, 55.84374999904394343, -5.000000000000103029 ) ) ;
#4932 = ADVANCED_FACE ( 'NONE', ( #9744 ), #1298, .F. ) ;
#4933 = CARTESIAN_POINT ( 'NONE',  ( -4.197393957002303999, -7.773935952363655451E-14, -3.503767560748929810 ) ) ;
#4934 = DIRECTION ( 'NONE',  ( 0.000000000000000000, 0.000000000000000000, 1.000000000000000000 ) ) ;
#4935 = EDGE_LOOP ( 'NONE', ( #10605, #3629, #5753, #3786 ) ) ;
#4936 = CIRCLE ( 'NONE', #7766, 3.499999999999997780 ) ;
#4937 = VECTOR ( 'NONE', #4338, 1000.000000000000000 ) ;
#4938 = CARTESIAN_POINT ( 'NONE',  ( 2.474873734152922111, 27.52512626584708144, 15.68750000000000355 ) ) ;
#4939 = CARTESIAN_POINT ( 'NONE',  ( -27.98076211353308551, 50.54999999999986926, -5.000000000000103029 ) ) ;
#4940 = CARTESIAN_POINT ( 'NONE',  ( -24.35964822603314772, 51.35208333237727629, -5.935950539335252074 ) ) ;
#4941 = CARTESIAN_POINT ( 'NONE',  ( -26.79131905728310059, 52.28541666571062052, -3.596074190997381237 ) ) ;
#4942 = VECTOR ( 'NONE', #1791, 1000.000000000000114 ) ;
#4943 = B_SPLINE_CURVE_WITH_KNOTS ( 'NONE', 3,
 ( #10370, #1260, #8819, #3811, #5431, #7934, #357, #3706, #251, #199 ),
 .UNSPECIFIED., .F., .F.,
 ( 4, 2, 2, 2, 4 ),
 ( 0.001590949097579384165, 0.001988361050532979398, 0.002385773003486574631, 0.002783184956440169864, 0.003180596909393765097 ),
 .UNSPECIFIED. ) ;
#4944 = PRESENTATION_LAYER_ASSIGNMENT (  '', '', ( #3164 ) ) ;
#4945 = CARTESIAN_POINT ( 'NONE',  ( 19.69775075566884226, 17.43975236193677603, 12.00579112326941988 ) ) ;
#4946 = CARTESIAN_POINT ( 'NONE',  ( -26.98076211353309972, 52.76666666666653072, -3.267949192431252037 ) ) ;
#4947 = ORIENTED_EDGE ( 'NONE', *, *, #4841, .F. ) ;
#4948 = DIRECTION ( 'NONE',  ( -1.000000000000000000, -0.000000000000000000, -0.000000000000000000 ) ) ;
#4949 = VERTEX_POINT ( 'NONE', #4142 ) ;
#4950 = ORIENTED_EDGE ( 'NONE', *, *, #4180, .F. ) ;
#4951 = CARTESIAN_POINT ( 'NONE',  ( 19.86292016999849608, 19.38279280778333202, 11.97810781016083403 ) ) ;
#4952 = ORIENTED_EDGE ( 'NONE', *, *, #9594, .T. ) ;
#4953 = STYLED_ITEM ( 'NONE', ( #6086 ), #5541 ) ;
#4954 = CARTESIAN_POINT ( 'NONE',  ( 5.000000000000004441, 0.000000000000000000, 0.000000000000000000 ) ) ;
#4955 = VERTEX_POINT ( 'NONE', #2538 ) ;
#4956 = CIRCLE ( 'NONE', #6368, 4.000000000000000000 ) ;
#4957 = CARTESIAN_POINT ( 'NONE',  ( 17.13192716875488131, 17.81782029955189728, 12.12541829646253078 ) ) ;
#4958 =( NAMED_UNIT ( * ) PLANE_ANGLE_UNIT ( ) SI_UNIT ( $, .RADIAN. ) );
#4959 = CARTESIAN_POINT ( 'NONE',  ( -31.74999999999995737, 2.449293598294707893E-16, -2.000000000000000888 ) ) ;
#4960 = CARTESIAN_POINT ( 'NONE',  ( 18.11095311068464397, 15.98247068297658835, 13.00034071860445550 ) ) ;
#4961 = EDGE_CURVE ( 'NONE', #318, #9904, #463, .T. ) ;
#4962 = CARTESIAN_POINT ( 'NONE',  ( -26.98076211353309972, 53.37916666475469896, -3.267949192431252037 ) ) ;
#4963 = CARTESIAN_POINT ( 'NONE',  ( -27.98076211353308551, 53.34999999999985931, -5.000000000000103029 ) ) ;
#4964 = CARTESIAN_POINT ( 'NONE',  ( -26.51666049839535688, 51.01876073720499960, -7.000000000000074607 ) ) ;
#4965 = ORIENTED_EDGE ( 'NONE', *, *, #3552, .T. ) ;
#4966 = CARTESIAN_POINT ( 'NONE',  ( -2.428085025993355295, 32.52166244231248271, 17.31030841526694175 ) ) ;
#4967 = EDGE_LOOP ( 'NONE', ( #8207, #2372, #2809, #9753, #9597, #495, #5345, #4478, #1381, #9121, #10111, #1067, #1112, #7707, #9001 ) ) ;
#4968 = CARTESIAN_POINT ( 'NONE',  ( 18.68606934758710025, 15.93178998805769453, 12.97541080761745924 ) ) ;
#4969 = PLANE ( 'NONE',  #10034 ) ;
#4970 = LINE ( 'NONE', #4122, #9736 ) ;
#4971 = LINE ( 'NONE', #9023, #3931 ) ;
#4972 = CARTESIAN_POINT ( 'NONE',  ( -1.814555661125939912, 31.72097824480680117, 14.06469158473306358 ) ) ;
#4973 = DIRECTION ( 'NONE',  ( -1.000000000000000000, 0.000000000000000000, 0.000000000000000000 ) ) ;
#4974 = ORIENTED_EDGE ( 'NONE', *, *, #3897, .T. ) ;
#4975 = CARTESIAN_POINT ( 'NONE',  ( 3.060260095956242488, 1.362955318038574948, 3.500000000000000000 ) ) ;
#4976 = VERTEX_POINT ( 'NONE', #6633 ) ;
#4977 = ORIENTED_EDGE ( 'NONE', *, *, #3630, .F. ) ;
#4978 = DIRECTION ( 'NONE',  ( 1.000000000000000000, -0.000000000000000000, -0.000000000000000000 ) ) ;
#4979 = CARTESIAN_POINT ( 'NONE',  ( -27.98076211353308551, 54.66249999808803040, -5.000000000000103029 ) ) ;
#4980 = CARTESIAN_POINT ( 'NONE',  ( 19.35452611835372849, 17.20101589911864437, 12.00579185514580338 ) ) ;
#4981 = CARTESIAN_POINT ( 'NONE',  ( 4.211140560182196957, 2.431303136016536470, -3.745885042887433514 ) ) ;
#4982 = CARTESIAN_POINT ( 'NONE',  ( 34.82458596820517016, 3.503579405888651799, 2.892497030208067699 ) ) ;
#4983 = CARTESIAN_POINT ( 'NONE',  ( -26.79131905728310059, 55.72708333237728340, -6.403925809002825709 ) ) ;
#4984 = CARTESIAN_POINT ( 'NONE',  ( 2.000000000000000000, 1.773042676681340524, -2.059984127722458425E-15 ) ) ;
#4985 = FACE_OUTER_BOUND ( 'NONE', #7211, .T. ) ;
#4986 = ORIENTED_EDGE ( 'NONE', *, *, #1832, .T. ) ;
#4987 = DIRECTION ( 'NONE',  ( -0.000000000000000000, -0.000000000000000000, 1.000000000000000000 ) ) ;
#4988 = CARTESIAN_POINT ( 'NONE',  ( 2.500000000000000000, 0.000000000000000000, 0.000000000000000000 ) ) ;
#4989 =( BOUNDED_SURFACE ( )  B_SPLINE_SURFACE ( 3, 2, ( 
 ( #6867, #2484, #10261, #5868, #692, #7476, #3255, #1591, #2425, #5042, #9199, #8362, #742, #1082, #5212, #9584, #8755, #2826, #1136, #3594, #9640, #8648, #1030, #4543, #249, #6981, #10317, #4441, #5320, #1934, #10368, #6247, #2034, #5265, #6307, #2712, #1818, #5370, #8704, #10536, #1984 ),
 ( #2931, #6197, #7764, #2766, #10427, #7931, #306, #3647, #3702, #4492, #7875, #10483, #7822, #7042, #7092, #2875, #5427, #8815, #1195, #3755, #8590, #4602, #9476, #6143, #196, #974, #9533, #7984, #7140, #354, #1871, #6087, #4380, #145, #3545, #6928, #669, #5783, #5682, #10067, #10593 ),
 ( #717, #4067, #7451, #10893, #5487, #406, #2393, #9060, #3807, #7197, #1506, #10840, #1455, #4006, #3227, #4650, #9169, #9756, #7505, #1257, #4848, #6604, #3346, #8222, #10005, #610, #1565, #7394, #8033, #8874, #9700, #4910, #769, #4118, #10786, #1620, #4966, #6668, #2987, #6367, #2148 ),
 ( #8282, #3174, #6557, #5843, #9954, #2339, #9226, #8337, #5731, #8393, #3285, #9109, #2460, #5018, #4175, #7564, #10952, #2094, #10290, #2634, #3400, #10122, #9449, #5075, #5294, #6010, #8454, #1002, #6953, #6841, #2684, #6782, #3460, #5133, #1906, #3516, #2568, #890, #10235, #10342, #7682 ),
 ( #5236, #2509, #220, #4466, #116, #6729, #9395, #1793, #7799, #5183, #946, #4239, #8563, #8682, #4349, #57, #8623, #4414, #5896, #173, #1056, #7737, #6905, #6060, #7848, #8511, #9281, #2736, #4293, #1674, #1843, #7625, #5953, #835, #1011, #3569, #6110, #9506, #10178, #9342, #1737 ),
 ( #4677, #10397, #5344, #7166, #10459, #8730, #1110, #6273, #8843, #6224, #8779, #1229, #9562, #2959, #3675, #1284, #6173, #9611, #4626, #8113, #2010, #3785, #2853, #10562, #5396, #1962, #2796, #3618, #9668, #5563, #8895, #1166, #6390, #5454, #434, #4514, #279, #7900, #8055, #4569, #2064 ),
 ( #10618, #7956, #7069, #3012, #8010, #333, #2171, #382, #3728, #7116, #3837, #6332, #9779, #9726, #10512, #2124, #2904, #5511, #7006, #7221, #8944, #1335, #4735, #2223, #5770, #704, #595, #7436, #540, #8213, #9890, #6649, #8270, #7326, #5672, #3991, #4105, #1442, #9212, #1606, #8325 ) ),
 .UNSPECIFIED., .T., .F., .F. ) 
 B_SPLINE_SURFACE_WITH_KNOTS ( ( 4, 3, 4 ),
 ( 3, 2, 2, 2, 2, 2, 2, 2, 2, 2, 2, 2, 2, 2, 2, 2, 2, 2, 2, 2, 3 ),
 ( 0.000000000000000000, 0.5000000000000000000, 1.000000000000000000 ),
 ( 0.000000000000000000, 0.04166666666666666435, 0.08333333333333332871, 0.1250000000000000000, 0.1666666666666666574, 0.2083333333333333426, 0.2500000000000000000, 0.2916666666666666852, 0.3333333333333333148, 0.3750000000000000000, 0.4166666666666666852, 0.4583333333333333148, 0.5000000000000000000, 0.5416666666666666297, 0.5833333333333333703, 0.6250000000000000000, 0.6666666666666666297, 0.7083333333333333703, 0.7500000000000000000, 0.7916666666666666297, 0.8001047462599640836 ),
 .UNSPECIFIED. ) 
 GEOMETRIC_REPRESENTATION_ITEM ( )  RATIONAL_B_SPLINE_SURFACE ( (
 ( 1.000000000000000000, 0.9238795325112867385, 1.000000000000000000, 0.9238795325112867385, 1.000000000000000000, 0.9238795325112867385, 1.000000000000000000, 0.9238795325112867385, 1.000000000000000000, 0.9238795325112867385, 1.000000000000000000, 0.9238795325112867385, 1.000000000000000000, 0.9238795325112867385, 1.000000000000000000, 0.9238795325112867385, 1.000000000000000000, 0.9238795325112867385, 1.000000000000000000, 0.9238795325112867385, 1.000000000000000000, 0.9238795325112867385, 1.000000000000000000, 0.9238795325112867385, 1.000000000000000000, 0.9238795325112867385, 1.000000000000000000, 0.9238795325112867385, 1.000000000000000000, 0.9238795325112867385, 1.000000000000000000, 0.9238795325112867385, 1.000000000000000000, 0.9238795325112867385, 1.000000000000000000, 0.9238795325112867385, 1.000000000000000000, 0.9238795325112867385, 1.000000000000000000, 0.9845845464796294522, 0.9754127805002987817),
 ( 0.3333333333333333703, 0.3079598441704289313, 0.3333333333333333703, 0.3079598441704289313, 0.3333333333333333703, 0.3079598441704289313, 0.3333333333333333703, 0.3079598441704289313, 0.3333333333333333703, 0.3079598441704289313, 0.3333333333333333703, 0.3079598441704289313, 0.3333333333333333703, 0.3079598441704289313, 0.3333333333333333703, 0.3079598441704289313, 0.3333333333333333703, 0.3079598441704289313, 0.3333333333333333703, 0.3079598441704289313, 0.3333333333333333703, 0.3079598441704289313, 0.3333333333333333703, 0.3079598441704289313, 0.3333333333333333703, 0.3079598441704289313, 0.3333333333333333703, 0.3079598441704289313, 0.3333333333333333703, 0.3079598441704289313, 0.3333333333333333703, 0.3079598441704289313, 0.3333333333333333703, 0.3079598441704289313, 0.3333333333333333703, 0.3079598441704289313, 0.3333333333333333703, 0.3079598441704289313, 0.3333333333333333703, 0.3281948488265432062, 0.3251375935000996309),
 ( 0.3333333333333333703, 0.3079598441704289313, 0.3333333333333333703, 0.3079598441704289313, 0.3333333333333333703, 0.3079598441704289313, 0.3333333333333333703, 0.3079598441704289313, 0.3333333333333333703, 0.3079598441704289313, 0.3333333333333333703, 0.3079598441704289313, 0.3333333333333333703, 0.3079598441704289313, 0.3333333333333333703, 0.3079598441704289313, 0.3333333333333333703, 0.3079598441704289313, 0.3333333333333333703, 0.3079598441704289313, 0.3333333333333333703, 0.3079598441704289313, 0.3333333333333333703, 0.3079598441704289313, 0.3333333333333333703, 0.3079598441704289313, 0.3333333333333333703, 0.3079598441704289313, 0.3333333333333333703, 0.3079598441704289313, 0.3333333333333333703, 0.3079598441704289313, 0.3333333333333333703, 0.3079598441704289313, 0.3333333333333333703, 0.3079598441704289313, 0.3333333333333333703, 0.3079598441704289313, 0.3333333333333333703, 0.3281948488265432062, 0.3251375935000996309),
 ( 1.000000000000000000, 0.9238795325112867385, 1.000000000000000000, 0.9238795325112867385, 1.000000000000000000, 0.9238795325112867385, 1.000000000000000000, 0.9238795325112867385, 1.000000000000000000, 0.9238795325112867385, 1.000000000000000000, 0.9238795325112867385, 1.000000000000000000, 0.9238795325112867385, 1.000000000000000000, 0.9238795325112867385, 1.000000000000000000, 0.9238795325112867385, 1.000000000000000000, 0.9238795325112867385, 1.000000000000000000, 0.9238795325112867385, 1.000000000000000000, 0.9238795325112867385, 1.000000000000000000, 0.9238795325112867385, 1.000000000000000000, 0.9238795325112867385, 1.000000000000000000, 0.9238795325112867385, 1.000000000000000000, 0.9238795325112867385, 1.000000000000000000, 0.9238795325112867385, 1.000000000000000000, 0.9238795325112867385, 1.000000000000000000, 0.9238795325112867385, 1.000000000000000000, 0.9845845464796294522, 0.9754127805002987817),
 ( 0.3333333333333333703, 0.3079598441704289313, 0.3333333333333333703, 0.3079598441704289313, 0.3333333333333333703, 0.3079598441704289313, 0.3333333333333333703, 0.3079598441704289313, 0.3333333333333333703, 0.3079598441704289313, 0.3333333333333333703, 0.3079598441704289313, 0.3333333333333333703, 0.3079598441704289313, 0.3333333333333333703, 0.3079598441704289313, 0.3333333333333333703, 0.3079598441704289313, 0.3333333333333333703, 0.3079598441704289313, 0.3333333333333333703, 0.3079598441704289313, 0.3333333333333333703, 0.3079598441704289313, 0.3333333333333333703, 0.3079598441704289313, 0.3333333333333333703, 0.3079598441704289313, 0.3333333333333333703, 0.3079598441704289313, 0.3333333333333333703, 0.3079598441704289313, 0.3333333333333333703, 0.3079598441704289313, 0.3333333333333333703, 0.3079598441704289313, 0.3333333333333333703, 0.3079598441704289313, 0.3333333333333333703, 0.3281948488265432062, 0.3251375935000996309),
 ( 0.3333333333333333703, 0.3079598441704289313, 0.3333333333333333703, 0.3079598441704289313, 0.3333333333333333703, 0.3079598441704289313, 0.3333333333333333703, 0.3079598441704289313, 0.3333333333333333703, 0.3079598441704289313, 0.3333333333333333703, 0.3079598441704289313, 0.3333333333333333703, 0.3079598441704289313, 0.3333333333333333703, 0.3079598441704289313, 0.3333333333333333703, 0.3079598441704289313, 0.3333333333333333703, 0.3079598441704289313, 0.3333333333333333703, 0.3079598441704289313, 0.3333333333333333703, 0.3079598441704289313, 0.3333333333333333703, 0.3079598441704289313, 0.3333333333333333703, 0.3079598441704289313, 0.3333333333333333703, 0.3079598441704289313, 0.3333333333333333703, 0.3079598441704289313, 0.3333333333333333703, 0.3079598441704289313, 0.3333333333333333703, 0.3079598441704289313, 0.3333333333333333703, 0.3079598441704289313, 0.3333333333333333703, 0.3281948488265432062, 0.3251375935000996309),
 ( 1.000000000000000000, 0.9238795325112867385, 1.000000000000000000, 0.9238795325112867385, 1.000000000000000000, 0.9238795325112867385, 1.000000000000000000, 0.9238795325112867385, 1.000000000000000000, 0.9238795325112867385, 1.000000000000000000, 0.9238795325112867385, 1.000000000000000000, 0.9238795325112867385, 1.000000000000000000, 0.9238795325112867385, 1.000000000000000000, 0.9238795325112867385, 1.000000000000000000, 0.9238795325112867385, 1.000000000000000000, 0.9238795325112867385, 1.000000000000000000, 0.9238795325112867385, 1.000000000000000000, 0.9238795325112867385, 1.000000000000000000, 0.9238795325112867385, 1.000000000000000000, 0.9238795325112867385, 1.000000000000000000, 0.9238795325112867385, 1.000000000000000000, 0.9238795325112867385, 1.000000000000000000, 0.9238795325112867385, 1.000000000000000000, 0.9238795325112867385, 1.000000000000000000, 0.9845845464796294522, 0.9754127805002987817) ) ) 
 REPRESENTATION_ITEM ( '' )  SURFACE ( )  );
#4990 = EDGE_CURVE ( 'NONE', #1598, #4566, #8965, .T. ) ;
#4991 = CARTESIAN_POINT ( 'NONE',  ( -26.79131905728310059, 50.12708333237728198, -6.403925809002825709 ) ) ;
#4992 = CARTESIAN_POINT ( 'NONE',  ( -26.79131905728310059, 54.38541666571061484, -3.596074190997381237 ) ) ;
#4993 = AXIS2_PLACEMENT_3D ( 'NONE', #9133, #8247, #1641 ) ;
#4994 = CARTESIAN_POINT ( 'NONE',  ( 22.03595509826854126, 19.06622527062933870, 12.00579112326941988 ) ) ;
#4995 = CARTESIAN_POINT ( 'NONE',  ( -27.98076211353308551, 52.59166666666653356, -6.154700538379338504 ) ) ;
#4996 = EDGE_LOOP ( 'NONE', ( #10275, #4289, #9183, #1653 ) ) ;
#4997 =( LENGTH_UNIT ( ) NAMED_UNIT ( * ) SI_UNIT ( .MILLI., .METRE. ) );
#4998 = ORIENTED_EDGE ( 'NONE', *, *, #9929, .T. ) ;
#4999 = ORIENTED_EDGE ( 'NONE', *, *, #3198, .F. ) ;
#5000 = LINE ( 'NONE', #8375, #3453 ) ;
#5001 = ORIENTED_EDGE ( 'NONE', *, *, #4536, .F. ) ;
#5002 = EDGE_CURVE ( 'NONE', #6726, #10201, #2770, .T. ) ;
#5003 = FACE_OUTER_BOUND ( 'NONE', #5087, .T. ) ;
#5004 = VERTEX_POINT ( 'NONE', #30 ) ;
#5005 = CARTESIAN_POINT ( 'NONE',  ( 22.78377297911024257, 19.69285065907503807, 11.00732503135576401 ) ) ;
#5006 =( NAMED_UNIT ( * ) PLANE_ANGLE_UNIT ( ) SI_UNIT ( $, .RADIAN. ) );
#5007 = CARTESIAN_POINT ( 'NONE',  ( 25.98076211353324183, 54.99999999999984368, 2.500000000000000000 ) ) ;
#5008 = CARTESIAN_POINT ( 'NONE',  ( 3.061158938895391923, -3.710337782248029015, 0.5735064479040067331 ) ) ;
#5009 = EDGE_CURVE ( 'NONE', #281, #9093, #6475, .T. ) ;
#5010 = CARTESIAN_POINT ( 'NONE',  ( 15.64372318925989802, 17.89181071667436385, 12.19867189564230969 ) ) ;
#5011 = CARTESIAN_POINT ( 'NONE',  ( 4.000000000000000000, 0.1981133338132474442, 2.382280164152719704E-17 ) ) ;
#5012 = CARTESIAN_POINT ( 'NONE',  ( -23.98076211353314235, 54.95416666475470180, -3.845299461620867554 ) ) ;
#5013 = CARTESIAN_POINT ( 'NONE',  ( -25.98076211353324894, 16.50000000000026290, -7.149999999999992362 ) ) ;
#5014 = ORIENTED_EDGE ( 'NONE', *, *, #6831, .F. ) ;
#5015 = LINE ( 'NONE', #8391, #1384 ) ;
#5016 = PRODUCT ( 'domed cap nut_din_DIN 1587 - M4 --NNU', 'domed cap nut_din_DIN 1587 - M4 --NNU', '', ( #8715 ) ) ;
#5017 = ORIENTED_EDGE ( 'NONE', *, *, #305, .F. ) ;
#5018 = CARTESIAN_POINT ( 'NONE',  ( 3.500000000000007994, 28.55025253169416644, 14.51562500000000355 ) ) ;
#5019 = CIRCLE ( 'NONE', #6783, 1.500000000000001332 ) ;
#5020 = ORIENTED_EDGE ( 'NONE', *, *, #6532, .F. ) ;
#5021 = CARTESIAN_POINT ( 'NONE',  ( 17.07425424873056130, 16.47910233548095604, 13.06769463237219320 ) ) ;
#5022 = ADVANCED_FACE ( 'NONE', ( #10151, #7478, #8363 ), #7596, .T. ) ;
#5023 = CARTESIAN_POINT ( 'NONE',  ( 19.36223501247343393, 16.11237126175916501, 11.95718771041564210 ) ) ;
#5024 = DIRECTION ( 'NONE',  ( 1.000000000000000000, -0.000000000000000000, -0.000000000000000000 ) ) ;
#5025 = AXIS2_PLACEMENT_3D ( 'NONE', #4114, #10118, #8389 ) ;
#5026 = DIRECTION ( 'NONE',  ( 0.000000000000000000, 0.000000000000000000, -1.000000000000000000 ) ) ;
#5027 = CARTESIAN_POINT ( 'NONE',  ( 0.9693646802875628410, 32.52740819067395961, 15.08031658473306891 ) ) ;
#5028 = CARTESIAN_POINT ( 'NONE',  ( -25.98076211353311393, 51.68749999808803608, -7.000000000000073719 ) ) ;
#5029 = FACE_OUTER_BOUND ( 'NONE', #9394, .T. ) ;
#5030 = ORIENTED_EDGE ( 'NONE', *, *, #953, .F. ) ;
#5031 = ORIENTED_EDGE ( 'NONE', *, *, #3824, .T. ) ;
#5032 = CARTESIAN_POINT ( 'NONE',  ( 0.1999999999999987899, 4.286263797015736595E-16, -3.500000000000000000 ) ) ;
#5033 = CARTESIAN_POINT ( 'NONE',  ( -4.000000000000000000, -1.680117682357936904, -3.316611593218794951 ) ) ;
#5034 = CARTESIAN_POINT ( 'NONE',  ( 34.99999999999999289, -7.999999999999996447, 17.50000000000000355 ) ) ;
#5035 = CARTESIAN_POINT ( 'NONE',  ( -23.98076211353314235, 55.71249999808803466, -5.000000000000103029 ) ) ;
#5036 = FACE_OUTER_BOUND ( 'NONE', #5547, .T. ) ;
#5037 = CARTESIAN_POINT ( 'NONE',  ( -26.79131905728310059, 50.88541666571061484, -3.596074190997381237 ) ) ;
#5038 = DIRECTION ( 'NONE',  ( -1.000000000000000000, 0.000000000000000000, 0.000000000000000000 ) ) ;
#5039 = CARTESIAN_POINT ( 'NONE',  ( 26.17691601781025312, 59.99615088301337096, 2.500000000000000000 ) ) ;
#5040 = VERTEX_POINT ( 'NONE', #9200 ) ;
#5041 =( BOUNDED_CURVE ( )  B_SPLINE_CURVE ( 2, ( #7363, #3923, #7308, #10544, #7205, #4660, #9871 ),
 .UNSPECIFIED., .F., .F. ) 
 B_SPLINE_CURVE_WITH_KNOTS ( ( 3, 2, 2, 3 ),
 ( 0.9166666666666667407, 0.9259259259259259300, 0.9444444444444444198, 0.9524110019352027834 ),
 .UNSPECIFIED. ) 
 CURVE ( )  GEOMETRIC_REPRESENTATION_ITEM ( )  RATIONAL_B_SPLINE_CURVE ( ( 0.9330127018922194093, 0.9330127018922197424, 1.000000000000000000, 0.8660254037844387076, 1.000000000000000000, 0.9423649185551699059, 0.9343183816103359796 ) ) 
 REPRESENTATION_ITEM ( '' )  );
#5042 = CARTESIAN_POINT ( 'NONE',  ( -1.035533905932736420, 27.49999999999998934, 14.20312500000000355 ) ) ;
#5043 = EDGE_CURVE ( 'NONE', #233, #7995, #3315, .T. ) ;
#5044 = CARTESIAN_POINT ( 'NONE',  ( -4.000000000000000000, -2.309401076758512694, -5.000000000000000000 ) ) ;
#5045 = CARTESIAN_POINT ( 'NONE',  ( -26.79131905728310059, 55.72708333237728340, -6.403925809002825709 ) ) ;
#5046 = AXIS2_PLACEMENT_3D ( 'NONE', #8491, #752, #10162 ) ;
#5047 = CARTESIAN_POINT ( 'NONE',  ( -27.44132332507749794, 55.71836679508493262, -4.296600267573891685 ) ) ;
#5048 = CARTESIAN_POINT ( 'NONE',  ( 34.99999999999999289, -3.999999999999993339, -4.999999999999995559 ) ) ;
#5049 = CARTESIAN_POINT ( 'NONE',  ( -23.98076211353314235, 51.54166666666652219, -3.845299461620867554 ) ) ;
#5050 = ORIENTED_EDGE ( 'NONE', *, *, #9052, .T. ) ;
#5051 = EDGE_CURVE ( 'NONE', #4811, #8576, #10945, .T. ) ;
#5052 = EDGE_LOOP ( 'NONE', ( #7337, #3033, #4977, #1066 ) ) ;
#5053 = CIRCLE ( 'NONE', #1677, 4.250000000000000000 ) ;
#5054 = VERTEX_POINT ( 'NONE', #918 ) ;
#5055 = DIRECTION ( 'NONE',  ( 0.000000000000000000, 0.000000000000000000, 1.000000000000000000 ) ) ;
#5056 = EDGE_LOOP ( 'NONE', ( #3215, #7056 ) ) ;
#5057 = EDGE_CURVE ( 'NONE', #990, #6444, #7652, .T. ) ;
#5058 = LINE ( 'NONE', #930, #7347 ) ;
#5059 = VERTEX_POINT ( 'NONE', #865 ) ;
#5060 = CARTESIAN_POINT ( 'NONE',  ( 22.26413902940654665, 19.29239618210221607, 11.00732503135576401 ) ) ;
#5061 = DIRECTION ( 'NONE',  ( 0.000000000000000000, -1.000000000000000000, 0.000000000000000000 ) ) ;
#5062 = CIRCLE ( 'NONE', #257, 0.2500000000000002220 ) ;
#5063 = DIRECTION ( 'NONE',  ( -1.000000000000000000, -0.000000000000000000, -0.000000000000000000 ) ) ;
#5064 = VECTOR ( 'NONE', #3448, 1000.000000000000000 ) ;
#5065 = CARTESIAN_POINT ( 'NONE',  ( -27.60187600103308014, 50.30208333237727913, -4.064049460664955760 ) ) ;
#5066 = CARTESIAN_POINT ( 'NONE',  ( 19.72987285752124720, 16.32873191470754648, 10.95281372472358861 ) ) ;
#5067 = EDGE_CURVE ( 'NONE', #3195, #3312, #6522, .T. ) ;
#5068 = CARTESIAN_POINT ( 'NONE',  ( -24.35964822603314772, 49.95208333237727771, -5.935950539335252074 ) ) ;
#5069 = AXIS2_PLACEMENT_3D ( 'NONE', #2786, #1784, #6160 ) ;
#5070 = DIRECTION ( 'NONE',  ( 0.000000000000000000, 0.000000000000000000, 1.000000000000000000 ) ) ;
#5071 = ORIENTED_EDGE ( 'NONE', *, *, #9052, .F. ) ;
#5072 = CARTESIAN_POINT ( 'NONE',  ( -27.98076211353308551, 50.40416666475469754, -6.154700538379338504 ) ) ;
#5073 = VERTEX_POINT ( 'NONE', #9423 ) ;
#5074 = VECTOR ( 'NONE', #6183, 1000.000000000000000 ) ;
#5075 = CARTESIAN_POINT ( 'NONE',  ( -3.500000000000002220, 28.55025253169416288, 15.29687500000000178 ) ) ;
#5076 = AXIS2_PLACEMENT_3D ( 'NONE', #7381, #7433, #1440 ) ;
#5077 = ORIENTED_EDGE ( 'NONE', *, *, #5988, .T. ) ;
#5078 = CARTESIAN_POINT ( 'NONE',  ( 16.47160909572790999, 17.06392481020577279, 13.12322671172946897 ) ) ;
#5079 = VECTOR ( 'NONE', #5362, 1000.000000000000000 ) ;
#5080 = CARTESIAN_POINT ( 'NONE',  ( -25.00815916299270825, 58.26638652017265940, -6.748499677373088979 ) ) ;
#5081 = CARTESIAN_POINT ( 'NONE',  ( 2.000000000000000000, 1.773042676681340524, -2.059984127722458425E-15 ) ) ;
#5082 = CARTESIAN_POINT ( 'NONE',  ( -25.17020516978313083, 51.70208333237728482, -3.596074190997380349 ) ) ;
#5083 = CARTESIAN_POINT ( 'NONE',  ( -2.500000000000005773, 29.99999999999999645, 13.96875000000000355 ) ) ;
#5084 = CARTESIAN_POINT ( 'NONE',  ( -25.98076211353311393, 51.33749999808802755, -3.000000000000132783 ) ) ;
#5085 = LINE ( 'NONE', #7807, #3114 ) ;
#5086 = CARTESIAN_POINT ( 'NONE',  ( 3.319999999999999840, 0.000000000000000000, 0.000000000000000000 ) ) ;
#5087 = EDGE_LOOP ( 'NONE', ( #5450, #2685, #5741, #8601, #1673 ) ) ;
#5088 = EDGE_LOOP ( 'NONE', ( #6408, #9938, #3875, #5466 ) ) ;
#5089 = CYLINDRICAL_SURFACE ( 'NONE', #6490, 1.999999999999971356 ) ;
#5090 = AXIS2_PLACEMENT_3D ( 'NONE', #9125, #10022, #2522 ) ;
#5091 = CARTESIAN_POINT ( 'NONE',  ( -4.000000000000000000, -2.309401076758512694, -3.433295621305382461 ) ) ;
#5092 = CARTESIAN_POINT ( 'NONE',  ( 19.05040816462259556, 17.06282649731835122, 12.00984920396035172 ) ) ;
#5093 = CARTESIAN_POINT ( 'NONE',  ( 1.767766952966372429, 31.76776695296637598, 14.75000000000000355 ) ) ;
#5094 = LINE ( 'NONE', #3139, #3576 ) ;
#5095 = CARTESIAN_POINT ( 'NONE',  ( -27.60187600103308014, 53.51041666571062194, -5.935950539335252074 ) ) ;
#5096 = DIRECTION ( 'NONE',  ( -1.000000000000000000, -0.000000000000000000, -0.000000000000000000 ) ) ;
#5097 = PLANE ( 'NONE',  #7906 ) ;
#5098 = CARTESIAN_POINT ( 'NONE',  ( 2.344047193898588954, 3.265465875126468021, -5.031375706690542042E-16 ) ) ;
#5099 = B_SPLINE_CURVE_WITH_KNOTS ( 'NONE', 3,
 ( #1556, #1611, #10171, #5008, #8330, #9160 ),
 .UNSPECIFIED., .F., .F.,
 ( 4, 2, 4 ),
 ( 0.002044882221487497216, 0.003063384235218479402, 0.004081886248949461587 ),
 .UNSPECIFIED. ) ;
#5100 = ORIENTED_EDGE ( 'NONE', *, *, #10099, .T. ) ;
#5101 = CARTESIAN_POINT ( 'NONE',  ( -30.75045812061784289, 13.49999999999941913, -9.500000000000000000 ) ) ;
#5102 = AXIS2_PLACEMENT_3D ( 'NONE', #2378, #7666, #7437 ) ;
#5103 = CARTESIAN_POINT ( 'NONE',  ( -1.999999999999999556, 3.464101615137754830, -3.142992957459232795 ) ) ;
#5104 = CARTESIAN_POINT ( 'NONE',  ( -27.60187600103308725, 52.40208333237728056, -4.064049460664955760 ) ) ;
#5105 = DIRECTION ( 'NONE',  ( -1.000000000000000000, -0.000000000000000000, -0.000000000000000000 ) ) ;
#5106 =( BOUNDED_CURVE ( )  B_SPLINE_CURVE ( 2, ( #7185, #9852, #10584, #6401, #9796, #2185, #5581, #1357, #10011 ),
 .UNSPECIFIED., .F., .F. ) 
 B_SPLINE_CURVE_WITH_KNOTS ( ( 3, 2, 2, 2, 3 ),
 ( 0.02777777777777775542, 0.03703703703703703498, 0.05555555555555555247, 0.07407407407407406996, 0.08333333333333331483 ),
 .UNSPECIFIED. ) 
 CURVE ( )  GEOMETRIC_REPRESENTATION_ITEM ( )  RATIONAL_B_SPLINE_CURVE ( ( 0.9330127018922194093, 0.9330127018922191873, 1.000000000000000000, 0.8660254037844387076, 1.000000000000000000, 0.8660254037844387076, 1.000000000000000000, 0.9330127018922194093, 0.9330127018922192983 ) ) 
 REPRESENTATION_ITEM ( '' )  );
#5107 = LINE ( 'NONE', #7659, #926 ) ;
#5108 = VECTOR ( 'NONE', #405, 1000.000000000000000 ) ;
#5109 =( GEOMETRIC_REPRESENTATION_CONTEXT ( 3 ) GLOBAL_UNCERTAINTY_ASSIGNED_CONTEXT ( ( #18 ) ) GLOBAL_UNIT_ASSIGNED_CONTEXT ( ( #5479, #8867, #10586 ) ) REPRESENTATION_CONTEXT ( 'NONE', 'WORKASPACE' ) );
#5110 = CARTESIAN_POINT ( 'NONE',  ( -27.98076211353308551, 54.10833333333319217, -3.845299461620869330 ) ) ;
#5111 = ORIENTED_EDGE ( 'NONE', *, *, #7191, .T. ) ;
#5112 = EDGE_LOOP ( 'NONE', ( #6618, #3593, #376 ) ) ;
#5113 = DIRECTION ( 'NONE',  ( 1.000000000000000000, 6.098637220230964906E-17, 0.000000000000000000 ) ) ;
#5114 = EDGE_LOOP ( 'NONE', ( #2497, #10874, #10577, #322, #1281, #9847 ) ) ;
#5115 = CYLINDRICAL_SURFACE ( 'NONE', #7718, 2.649999999999991029 ) ;
#5116 = SURFACE_STYLE_FILL_AREA ( #4278 ) ;
#5117 = ORIENTED_EDGE ( 'NONE', *, *, #3582, .T. ) ;
#5119 = CARTESIAN_POINT ( 'NONE',  ( 20.43380676890320657, 22.25420293214091316, 12.00579112326941988 ) ) ;
#5118 = VECTOR ( 'NONE', #4748, 1000.000000000000000 ) ;
#5120 = MECHANICAL_DESIGN_GEOMETRIC_PRESENTATION_REPRESENTATION (  '', ( #9013 ), #1756 ) ;
#5121 = DIRECTION ( 'NONE',  ( -1.000000000000000000, 0.000000000000000000, 0.000000000000000000 ) ) ;
#5122 = CARTESIAN_POINT ( 'NONE',  ( -26.98076211353309972, 51.74583333142136610, -6.732050807568954909 ) ) ;
#5123 = CARTESIAN_POINT ( 'NONE',  ( -23.98076211353314235, 50.11249999808803324, -5.000000000000103029 ) ) ;
#5124 = CARTESIAN_POINT ( 'NONE',  ( 22.86591953417209666, 18.42728137938113875, 11.95042449705224819 ) ) ;
#5125 = DIRECTION ( 'NONE',  ( 0.000000000000000000, 0.000000000000000000, -1.000000000000000000 ) ) ;
#5126 = CARTESIAN_POINT ( 'NONE',  ( -24.98076211353313170, 54.89583333142136468, -3.267949192431250705 ) ) ;
#5127 = AXIS2_PLACEMENT_3D ( 'NONE', #4522, #5461, #1914 ) ;
#5128 = DIRECTION ( 'NONE',  ( 0.000000000000000000, 1.000000000000000000, -1.224646799147353207E-16 ) ) ;
#5129 = ORIENTED_EDGE ( 'NONE', *, *, #6338, .T. ) ;
#5130 = DIRECTION ( 'NONE',  ( -0.000000000000000000, -0.000000000000000000, -1.000000000000000000 ) ) ;
#5131 = ORIENTED_EDGE ( 'NONE', *, *, #2967, .T. ) ;
#5132 = CONICAL_SURFACE ( 'NONE', #496, 1.535500000000000087, 1.047197551196590748 ) ;
#5133 = CARTESIAN_POINT ( 'NONE',  ( 1.449747468305833120, 33.50000000000000000, 16.07812500000000355 ) ) ;
#5134 = EDGE_LOOP ( 'NONE', ( #10655, #5180, #1337, #542 ) ) ;
#5135 = CARTESIAN_POINT ( 'NONE',  ( 15.69051189741946573, 17.84502200851479614, 13.19648031090924789 ) ) ;
#5136 = EDGE_CURVE ( 'NONE', #8126, #1456, #1592, .T. ) ;
#5137 = EDGE_CURVE ( 'NONE', #6171, #10078, #6114, .T. ) ;
#5138 = FACE_OUTER_BOUND ( 'NONE', #1752, .T. ) ;
#5139 = CARTESIAN_POINT ( 'NONE',  ( 19.77604874367146692, 21.01153129092389094, 12.00579112326941988 ) ) ;
#5140 = CARTESIAN_POINT ( 'NONE',  ( -27.60187600103308014, 50.12708333237727487, -4.064049460664955760 ) ) ;
#5141 = DIRECTION ( 'NONE',  ( -1.000000000000000000, 0.000000000000000000, 0.000000000000000000 ) ) ;
#5142 = LINE ( 'NONE', #8522, #7206 ) ;
#5143 = DIRECTION ( 'NONE',  ( 1.000000000000000000, -0.000000000000000000, -0.000000000000000000 ) ) ;
#5144 = DIRECTION ( 'NONE',  ( 0.000000000000000000, -1.807003620809174139E-16, -1.000000000000000000 ) ) ;
#5145 = ORIENTED_EDGE ( 'NONE', *, *, #3572, .F. ) ;
#5146 = EDGE_LOOP ( 'NONE', ( #5443, #3383 ) ) ;
#5147 = DIRECTION ( 'NONE',  ( 0.000000000000000000, 0.000000000000000000, -1.000000000000000000 ) ) ;
#5148 = EDGE_CURVE ( 'NONE', #7578, #4616, #3488, .T. ) ;
#5149 = CARTESIAN_POINT ( 'NONE',  ( -26.51666049839534978, 54.80623925897107540, -3.000000000000133227 ) ) ;
#5150 = CARTESIAN_POINT ( 'NONE',  ( 20.17304365239387565, 21.99495017005343200, 12.00579112326981068 ) ) ;
#5151 = CARTESIAN_POINT ( 'NONE',  ( 1.035533905932737975, 32.50000000000000711, 16.07812500000000355 ) ) ;
#5152 = CARTESIAN_POINT ( 'NONE',  ( 5.384454397937118664, 0.000000000000000000, -4.484454397937119197 ) ) ;
#5153 = CARTESIAN_POINT ( 'NONE',  ( -26.79131905728310059, 52.28541666571062052, -3.596074190997381237 ) ) ;
#5154 = CARTESIAN_POINT ( 'NONE',  ( -6.015568632492056977, 34.47916666666665009, 2.500000000000000000 ) ) ;
#5155 = CARTESIAN_POINT ( 'NONE',  ( 0.000000000000000000, 30.00000000000000000, 2.500000000000000000 ) ) ;
#5156 = DIRECTION ( 'NONE',  ( -0.000000000000000000, -0.000000000000000000, 1.000000000000000000 ) ) ;
#5157 = ORIENTED_EDGE ( 'NONE', *, *, #6469, .T. ) ;
#5158 = DIRECTION ( 'NONE',  ( 0.000000000000000000, 0.000000000000000000, -1.000000000000000000 ) ) ;
#5159 = DIRECTION ( 'NONE',  ( -1.000000000000000000, -0.000000000000000000, -0.000000000000000000 ) ) ;
#5160 = CARTESIAN_POINT ( 'NONE',  ( -24.35964822603314772, 54.15208333237727345, -5.935950539335252074 ) ) ;
#5161 = EDGE_CURVE ( 'NONE', #5523, #9017, #5347, .T. ) ;
#5162 = CARTESIAN_POINT ( 'NONE',  ( -24.98076211353312814, 51.01666666666653072, -6.732050807568954909 ) ) ;
#5163 = DIRECTION ( 'NONE',  ( 0.000000000000000000, -0.000000000000000000, 1.000000000000000000 ) ) ;
#5164 = CARTESIAN_POINT ( 'NONE',  ( -27.98076211353308551, 51.89166666666653782, -6.154700538379338504 ) ) ;
#5165 = VERTEX_POINT ( 'NONE', #7932 ) ;
#5166 = ORIENTED_EDGE ( 'NONE', *, *, #10355, .F. ) ;
#5167 = CARTESIAN_POINT ( 'NONE',  ( 0.03019833794501056504, 0.6882444255503935571, -3.500000000000000000 ) ) ;
#5168 = DIRECTION ( 'NONE',  ( 1.000000000000000000, -0.000000000000000000, 1.156482317317871478E-16 ) ) ;
#5169 = APPLICATION_PROTOCOL_DEFINITION ( 'draft international standard', 'automotive_design', 1998, #3230 ) ;
#5170 = ORIENTED_EDGE ( 'NONE', *, *, #1042, .T. ) ;
#5171 = DIRECTION ( 'NONE',  ( 0.000000000000000000, -1.000000000000000000, 0.000000000000000000 ) ) ;
#5172 = CARTESIAN_POINT ( 'NONE',  ( 0.000000000000000000, -1.178949249685213863, 2.042000000000002924 ) ) ;
#5173 = CARTESIAN_POINT ( 'NONE',  ( -26.98076211353309972, 51.97916666475470038, -3.267949192431252037 ) ) ;
#5174 = DIRECTION ( 'NONE',  ( 0.000000000000000000, 0.000000000000000000, 1.000000000000000000 ) ) ;
#5175 = CARTESIAN_POINT ( 'NONE',  ( 18.86745781575159242, 21.66267592685425569, 11.95042449705185561 ) ) ;
#5176 = CARTESIAN_POINT ( 'NONE',  ( 3.500000000000005773, 31.44974746830583001, 15.92187500000000178 ) ) ;
#5177 = CARTESIAN_POINT ( 'NONE',  ( -23.98076211353314235, 54.37083333142137320, -6.154700538379337615 ) ) ;
#5178 = CONICAL_SURFACE ( 'NONE', #7657, 2.767949192431121919, 0.5235987755982963732 ) ;
#5179 = CARTESIAN_POINT ( 'NONE',  ( -23.98076211353314235, 53.69999999999986784, -5.000000000000103029 ) ) ;
#5180 = ORIENTED_EDGE ( 'NONE', *, *, #10764, .T. ) ;
#5181 = CARTESIAN_POINT ( 'NONE',  ( -26.51666049839534622, 50.60623925897106545, -3.000000000000131006 ) ) ;
#5182 = VERTEX_POINT ( 'NONE', #3546 ) ;
#5183 = CARTESIAN_POINT ( 'NONE',  ( -1.383578242660655100, 26.47259180932604039, 13.20531658473306713 ) ) ;
#5184 = ORIENTED_EDGE ( 'NONE', *, *, #10658, .F. ) ;
#5185 = ADVANCED_FACE ( 'NONE', ( #9534 ), #8651, .F. ) ;
#5186 = CARTESIAN_POINT ( 'NONE',  ( 19.75845051886964043, 23.09045650430892849, 12.94889058896590583 ) ) ;
#5187 = CARTESIAN_POINT ( 'NONE',  ( 18.07012887690021330, 16.02595819568259827, 12.00212024154935975 ) ) ;
#5188 = CARTESIAN_POINT ( 'NONE',  ( 19.13264607096459002, 17.09257730534942965, 12.00833071292064425 ) ) ;
#5189 = CARTESIAN_POINT ( 'NONE',  ( -26.79131905728310059, 52.98541666571061626, -3.596074190997381237 ) ) ;
#5190 = CARTESIAN_POINT ( 'NONE',  ( -2.458860273309268152, 29.54350846364475203, 15.50141270685246830 ) ) ;
#5191 = CARTESIAN_POINT ( 'NONE',  ( 0.3126073911691312213, -2.020725942164384836, 3.499999999999999556 ) ) ;
#5192 = DIRECTION ( 'NONE',  ( 0.000000000000000000, -0.000000000000000000, 1.000000000000000000 ) ) ;
#5193 = ADVANCED_FACE ( 'NONE', ( #6088 ), #4544, .F. ) ;
#5194 = ORIENTED_EDGE ( 'NONE', *, *, #3633, .F. ) ;
#5195 = ORIENTED_EDGE ( 'NONE', *, *, #6672, .F. ) ;
#5196 = EDGE_CURVE ( 'NONE', #5966, #10907, #6304, .T. ) ;
#5197 = CARTESIAN_POINT ( 'NONE',  ( 17.79249663040192431, 17.21067465782413919, 12.06642298039558980 ) ) ;
#5198 = B_SPLINE_CURVE_WITH_KNOTS ( 'NONE', 3,
 ( #1776, #9380, #5167, #4330, #2669, #6044 ),
 .UNSPECIFIED., .F., .F.,
 ( 4, 2, 4 ),
 ( 0.005702039456357650346, 0.006725091618211351784, 0.007748143780065053221 ),
 .UNSPECIFIED. ) ;
#5200 = B_SPLINE_CURVE_WITH_KNOTS ( 'NONE', 3,
 ( #2649, #4131, #5797, #3415, #9186, #4923 ),
 .UNSPECIFIED., .F., .F.,
 ( 4, 2, 4 ),
 ( 0.002044882221487536681, 0.003063384235218498050, 0.004081886248949459853 ),
 .UNSPECIFIED. ) ;
#5199 = FACE_OUTER_BOUND ( 'NONE', #7579, .T. ) ;
#5201 = PRODUCT_DEFINITION_SHAPE ( 'NONE', 'NONE',  #8986 ) ;
#5202 = DIRECTION ( 'NONE',  ( 1.000000000000000000, 0.000000000000000000, 0.000000000000000000 ) ) ;
#5203 = VECTOR ( 'NONE', #178, 1000.000000000000000 ) ;
#5204 = CARTESIAN_POINT ( 'NONE',  ( -25.44486372867087454, 55.56876073720499676, -3.000000000000134559 ) ) ;
#5205 = CARTESIAN_POINT ( 'NONE',  ( -25.98076211353311393, 59.00000000000083134, -7.000000000000074607 ) ) ;
#5206 = CARTESIAN_POINT ( 'NONE',  ( -27.60187600103308370, 53.56874999904395196, -5.000000000000103029 ) ) ;
#5207 = CARTESIAN_POINT ( 'NONE',  ( 0.000000000000000000, 0.000000000000000000, 0.000000000000000000 ) ) ;
#5208 = CARTESIAN_POINT ( 'NONE',  ( -25.47250412700868338, 57.12887987407799528, -3.061742751175442923 ) ) ;
#5209 = CARTESIAN_POINT ( 'NONE',  ( 2.000000000000005329, -3.464101615137751722, 0.000000000000000000 ) ) ;
#5210 = ADVANCED_FACE ( 'NONE', ( #3648 ), #4925, .T. ) ;
#5211 = ORIENTED_EDGE ( 'NONE', *, *, #3089, .T. ) ;
#5212 = CARTESIAN_POINT ( 'NONE',  ( 2.500000000000008438, 30.00000000000000711, 14.59375000000000178 ) ) ;
#5213 = CARTESIAN_POINT ( 'NONE',  ( -26.51666049839534978, 54.19373926088289295, -3.000000000000133227 ) ) ;
#5214 = EDGE_CURVE ( 'NONE', #3160, #1491, #8485, .T. ) ;
#5215 = EDGE_CURVE ( 'NONE', #6853, #2434, #9457, .T. ) ;
#5216 = CARTESIAN_POINT ( 'NONE',  ( -26.79131905728310059, 52.22708333237727629, -6.403925809002825709 ) ) ;
#5217 = CARTESIAN_POINT ( 'NONE',  ( -24.35964822603314417, 55.31874999904395196, -5.000000000000103029 ) ) ;
#5218 = DIRECTION ( 'NONE',  ( 4.312387734421975126E-17, -0.7071067811865451302, 0.7071067811865500152 ) ) ;
#5219 = CARTESIAN_POINT ( 'NONE',  ( 0.000000000000000000, 4.163799117101000559E-16, -3.299999999999999822 ) ) ;
#5220 = EDGE_LOOP ( 'NONE', ( #5195, #1766, #6385, #9462 ) ) ;
#5221 = ORIENTED_EDGE ( 'NONE', *, *, #867, .F. ) ;
#5222 = DIRECTION ( 'NONE',  ( 1.000000000000000000, 6.098637220230963674E-17, -0.000000000000000000 ) ) ;
#5223 = DIRECTION ( 'NONE',  ( 0.000000000000000000, -1.000000000000000000, 0.000000000000000000 ) ) ;
#5224 = ORIENTED_EDGE ( 'NONE', *, *, #2396, .F. ) ;
#5225 = CARTESIAN_POINT ( 'NONE',  ( 21.90605485701305000, 18.97586566459109392, 12.00579112326941988 ) ) ;
#5226 = CARTESIAN_POINT ( 'NONE',  ( 1.411581201560190495E-15, 4.862606272033091592, -3.745885042887436622 ) ) ;
#5227 = CARTESIAN_POINT ( 'NONE',  ( 1.047444401652940007E-13, 30.00000000000000000, -2.500000000000000000 ) ) ;
#5228 = EDGE_CURVE ( 'NONE', #1168, #2458, #4359, .T. ) ;
#5229 = CARTESIAN_POINT ( 'NONE',  ( 15.59693448110033032, 17.93859942483392800, 11.20086348037537327 ) ) ;
#5230 = CYLINDRICAL_SURFACE ( 'NONE', #211, 2.500000000000000888 ) ;
#5231 = CARTESIAN_POINT ( 'NONE',  ( -25.17020516978313083, 50.47708333237727629, -3.596074190997380349 ) ) ;
#5232 = FACE_OUTER_BOUND ( 'NONE', #1971, .T. ) ;
#5233 = ORIENTED_EDGE ( 'NONE', *, *, #9761, .T. ) ;
#5234 = DIRECTION ( 'NONE',  ( 1.000000000000000000, -0.000000000000000000, -0.000000000000000000 ) ) ;
#5235 = ORIENTED_EDGE ( 'NONE', *, *, #6626, .F. ) ;
#5236 = CARTESIAN_POINT ( 'NONE',  ( 2.428085025993350410, 32.52166244231248271, 12.50219158473306358 ) ) ;
#5237 = AXIS2_PLACEMENT_3D ( 'NONE', #6984, #7879, #9703 ) ;
#5238 = ORIENTED_EDGE ( 'NONE', *, *, #302, .F. ) ;
#5239 = CARTESIAN_POINT ( 'NONE',  ( 24.03139851132786831, 19.63770821034670533, 11.95042449705224996 ) ) ;
#5240 = CIRCLE ( 'NONE', #2935, 7.500000000000000000 ) ;
#5241 = CARTESIAN_POINT ( 'NONE',  ( 24.09141472773967507, 22.06251279622207306, 11.95042449705264076 ) ) ;
#5242 = CARTESIAN_POINT ( 'NONE',  ( 0.2949799022107380542, 0.000000000000000000, 0.000000000000000000 ) ) ;
#5243 = CARTESIAN_POINT ( 'NONE',  ( -24.35964822603314772, 51.06041666571061199, -4.064049460664953983 ) ) ;
#5244 = AXIS2_PLACEMENT_3D ( 'NONE', #7058, #268, #2949 ) ;
#5245 = CARTESIAN_POINT ( 'NONE',  ( 2.500000000000008438, 30.00000000000000711, 15.84375000000000355 ) ) ;
#5246 = CONICAL_SURFACE ( 'NONE', #10913, 2.059999999999998721, 0.9599310885968738161 ) ;
#5247 = AXIS2_PLACEMENT_3D ( 'NONE', #6159, #266, #8717 ) ;
#5248 = FACE_OUTER_BOUND ( 'NONE', #2668, .T. ) ;
#5249 = LINE ( 'NONE', #848, #1541 ) ;
#5250 = ORIENTED_EDGE ( 'NONE', *, *, #5677, .T. ) ;
#5251 = ORIENTED_EDGE ( 'NONE', *, *, #9317, .F. ) ;
#5252 = DIRECTION ( 'NONE',  ( 0.000000000000000000, 1.000000000000000000, 0.000000000000000000 ) ) ;
#5253 = VECTOR ( 'NONE', #8922, 1000.000000000000000 ) ;
#5254 = CYLINDRICAL_SURFACE ( 'NONE', #3286, 1.999999999999971356 ) ;
#5255 = DIRECTION ( 'NONE',  ( 0.000000000000000000, -1.000000000000000000, 0.000000000000000000 ) ) ;
#5256 = AXIS2_PLACEMENT_3D ( 'NONE', #10600, #4772, #3767 ) ;
#5257 = CARTESIAN_POINT ( 'NONE',  ( -25.98076211353311393, 52.82499999999986784, -3.000000000000132339 ) ) ;
#5258 = CARTESIAN_POINT ( 'NONE',  ( 2.836893136758676270, 3.208949435745843903, -3.505054077164911241 ) ) ;
#5259 = CARTESIAN_POINT ( 'NONE',  ( -27.60187600103308014, 55.02708333237728056, -4.064049460664955760 ) ) ;
#5260 = CARTESIAN_POINT ( 'NONE',  ( 1.411581201560190495E-15, 4.862606272033091592, -3.745885042887436622 ) ) ;
#5261 = CARTESIAN_POINT ( 'NONE',  ( 29.49999999999999289, 2.000000000000001776, -12.50099999999999767 ) ) ;
#5262 = ORIENTED_EDGE ( 'NONE', *, *, #2738, .T. ) ;
#5263 = CARTESIAN_POINT ( 'NONE',  ( -26.98076211353309972, 54.07916666475470180, -3.267949192431252037 ) ) ;
#5264 = CIRCLE ( 'NONE', #8802, 4.250000000000000000 ) ;
#5265 = CARTESIAN_POINT ( 'NONE',  ( 1.035533905932737975, 32.50000000000000711, 16.07812500000000355 ) ) ;
#5266 = CARTESIAN_POINT ( 'NONE',  ( -1.767766952966370209, 28.23223304703362402, 14.12500000000000355 ) ) ;
#5267 = CARTESIAN_POINT ( 'NONE',  ( -25.98076211353310683, 53.91874999904394627, -3.128098921329806714 ) ) ;
#5268 = EDGE_CURVE ( 'NONE', #2494, #1437, #6961, .T. ) ;
#5269 = LINE ( 'NONE', #803, #3112 ) ;
#5270 = EDGE_CURVE ( 'NONE', #829, #6966, #5406, .T. ) ;
#5271 = MANIFOLD_SOLID_BREP ( 'Sweep2', #2214 ) ;
#5272 = AXIS2_PLACEMENT_3D ( 'NONE', #5525, #8907, #8023 ) ;
#5273 = CARTESIAN_POINT ( 'NONE',  ( -30.31088913245546124, 17.49999999999980815, -2.500000000000000000 ) ) ;
#5274 = LINE ( 'NONE', #8660, #7843 ) ;
#5275 = VERTEX_POINT ( 'NONE', #9514 ) ;
#5276 = ORIENTED_EDGE ( 'NONE', *, *, #1740, .F. ) ;
#5277 = FACE_OUTER_BOUND ( 'NONE', #3155, .T. ) ;
#5278 = DIRECTION ( 'NONE',  ( -1.000000000000000000, -0.000000000000000000, -0.000000000000000000 ) ) ;
#5279 = CARTESIAN_POINT ( 'NONE',  ( -25.98076211353233234, 49.50000000000063949, -4.999999999999622524 ) ) ;
#5280 = ORIENTED_EDGE ( 'NONE', *, *, #1583, .F. ) ;
#5281 = CARTESIAN_POINT ( 'NONE',  ( 6.098637220230963427E-16, -10.00000000000000000, 15.49999999999998934 ) ) ;
#5282 = LINE ( 'NONE', #8719, #2588 ) ;
#5283 = SHAPE_REPRESENTATION ( 'Cable Pinch Bolt Clamp', ( #308 ), #6179 ) ;
#5284 = CARTESIAN_POINT ( 'NONE',  ( 19.46525898981753855, 16.20608772750926718, 10.95621100456342312 ) ) ;
#5285 = CARTESIAN_POINT ( 'NONE',  ( -2.000000000000007550, -3.464101615137749945, 0.000000000000000000 ) ) ;
#5286 = CARTESIAN_POINT ( 'NONE',  ( -25.98076211353311393, 53.21874999904395054, -3.128098921329806714 ) ) ;
#5287 = CARTESIAN_POINT ( 'NONE',  ( 0.000000000000000000, 0.000000000000000000, 0.000000000000000000 ) ) ;
#5288 = ORIENTED_EDGE ( 'NONE', *, *, #10319, .T. ) ;
#5289 = DIRECTION ( 'NONE',  ( -0.000000000000000000, -0.000000000000000000, -1.000000000000000000 ) ) ;
#5290 = PRODUCT ( 'caliper arm left', 'caliper arm left', '', ( #1044 ) ) ;
#5291 = ORIENTED_EDGE ( 'NONE', *, *, #5967, .T. ) ;
#5292 = VECTOR ( 'NONE', #10723, 1000.000000000000000 ) ;
#5293 = CIRCLE ( 'NONE', #7584, 2.200000000000001066 ) ;
#5294 = CARTESIAN_POINT ( 'NONE',  ( -2.474873734152916338, 27.52512626584707789, 15.37500000000000355 ) ) ;
#5295 = ORIENTED_EDGE ( 'NONE', *, *, #555, .F. ) ;
#5296 = CARTESIAN_POINT ( 'NONE',  ( 18.64799062861727563, 15.97503555906617123, 11.97707131907271005 ) ) ;
#5297 = SURFACE_SIDE_STYLE ('',( #3621 ) ) ;
#5298 = EDGE_CURVE ( 'NONE', #947, #10068, #4418, .T. ) ;
#5299 = DIRECTION ( 'NONE',  ( 0.000000000000000000, 1.000000000000000000, 0.000000000000000000 ) ) ;
#5300 =( GEOMETRIC_REPRESENTATION_CONTEXT ( 3 ) GLOBAL_UNCERTAINTY_ASSIGNED_CONTEXT ( ( #3861 ) ) GLOBAL_UNIT_ASSIGNED_CONTEXT ( ( #4997, #6980, #1869 ) ) REPRESENTATION_CONTEXT ( 'NONE', 'WORKASPACE' ) );
#5301 = CARTESIAN_POINT ( 'NONE',  ( 16.11564427137601285, 18.83410319690818824, 12.22072830420661660 ) ) ;
#5302 = CARTESIAN_POINT ( 'NONE',  ( -25.17020516978313083, 51.23541666571061626, -6.403925809002825709 ) ) ;
#5303 = DIRECTION ( 'NONE',  ( 1.000000000000000000, -0.000000000000000000, -0.000000000000000000 ) ) ;
#5304 = LINE ( 'NONE', #1686, #1196 ) ;
#5305 = ORIENTED_EDGE ( 'NONE', *, *, #5051, .F. ) ;
#5306 = ORIENTED_EDGE ( 'NONE', *, *, #7454, .F. ) ;
#5307 = STYLED_ITEM ( 'NONE', ( #3034 ), #5578 ) ;
#5308 = LINE ( 'NONE', #344, #10230 ) ;
#5309 = LINE ( 'NONE', #6917, #9158 ) ;
#5310 = VECTOR ( 'NONE', #8287, 1000.000000000000000 ) ;
#5311 = FILL_AREA_STYLE_COLOUR ( '', #6459 ) ;
#5312 = CARTESIAN_POINT ( 'NONE',  ( -26.95345029339875609, 58.26591186299814495, -3.251555783389634247 ) ) ;
#5313 = CARTESIAN_POINT ( 'NONE',  ( -0.1756481739660520902, 4.720212674038980261, -3.469390959564065291 ) ) ;
#5314 = CARTESIAN_POINT ( 'NONE',  ( -27.60187600103308014, 52.81041666571061199, -5.935950539335252074 ) ) ;
#5315 = CARTESIAN_POINT ( 'NONE',  ( -23.98076211353314235, 49.55833333333319501, -6.154700538379337615 ) ) ;
#5316 = DIRECTION ( 'NONE',  ( 0.000000000000000000, 0.000000000000000000, 1.000000000000000000 ) ) ;
#5317 = CARTESIAN_POINT ( 'NONE',  ( 29.50000000000000711, 2.000000000000001776, 5.500000000000000000 ) ) ;
#5318 = VERTEX_POINT ( 'NONE', #8062 ) ;
#5319 = SURFACE_STYLE_FILL_AREA ( #972 ) ;
#5320 = CARTESIAN_POINT ( 'NONE',  ( 1.767766952966377314, 28.23223304703363112, 15.68750000000000355 ) ) ;
#5321 = CARTESIAN_POINT ( 'NONE',  ( -2.385244779468109755E-15, 32.50000000000000711, 13.65625000000000355 ) ) ;
#5322 = UNCERTAINTY_MEASURE_WITH_UNIT (LENGTH_MEASURE( 1.000000000000000082E-05 ), #3894, 'distance_accuracy_value', 'NONE');
#5323 = DIRECTION ( 'NONE',  ( 1.000000000000000000, -0.000000000000000000, -0.000000000000000000 ) ) ;
#5324 = CARTESIAN_POINT ( 'NONE',  ( -23.98076211353314235, 52.99999999999986500, -5.000000000000103029 ) ) ;
#5325 = DIRECTION ( 'NONE',  ( -1.000000000000000000, -6.098637220230964906E-17, -6.308085367188384325E-16 ) ) ;
#5326 = CARTESIAN_POINT ( 'NONE',  ( 0.000000000000000000, 0.000000000000000000, 0.000000000000000000 ) ) ;
#5327 = EDGE_LOOP ( 'NONE', ( #2986, #5909, #1655, #1153 ) ) ;
#5328 = ORIENTED_EDGE ( 'NONE', *, *, #2925, .T. ) ;
#5329 = CARTESIAN_POINT ( 'NONE',  ( 25.78460820925620922, 50.00384911698630930, 2.500000000000000000 ) ) ;
#5330 = EDGE_CURVE ( 'NONE', #4955, #10495, #7237, .T. ) ;
#5331 = LINE ( 'NONE', #5441, #3274 ) ;
#5332 = ORIENTED_EDGE ( 'NONE', *, *, #6636, .T. ) ;
#5333 = EDGE_CURVE ( 'NONE', #9782, #4079, #3736, .T. ) ;
#5334 = CARTESIAN_POINT ( 'NONE',  ( 34.99999999999987210, -3.999999999999989786, 9.999999999999998224 ) ) ;
#5335 = CARTESIAN_POINT ( 'NONE',  ( 25.98076211353311749, 56.49999999999984368, 12.14999999999999147 ) ) ;
#5336 = CARTESIAN_POINT ( 'NONE',  ( 21.48473758187327931, 18.75023854587115935, 11.00732503135576401 ) ) ;
#5337 = FACE_OUTER_BOUND ( 'NONE', #1844, .T. ) ;
#5338 = CARTESIAN_POINT ( 'NONE',  ( -24.35964822603314417, 52.69374999904394485, -5.000000000000103029 ) ) ;
#5339 = ADVANCED_FACE ( 'NONE', ( #6282 ), #1063, .F. ) ;
#5340 = CARTESIAN_POINT ( 'NONE',  ( 0.000000000000000000, 1.178949249685218525, 2.041999999999999371 ) ) ;
#5341 = ORIENTED_EDGE ( 'NONE', *, *, #9616, .F. ) ;
#5342 = LINE ( 'NONE', #331, #6887 ) ;
#5343 = ORIENTED_EDGE ( 'NONE', *, *, #6530, .F. ) ;
#5344 = CARTESIAN_POINT ( 'NONE',  ( -0.06616922564517727090, 32.50000000000000711, 12.65844158473306535 ) ) ;
#5345 = ORIENTED_EDGE ( 'NONE', *, *, #838, .F. ) ;
#5346 = CARTESIAN_POINT ( 'NONE',  ( 19.34072721801214456, 22.67515267995686656, 12.94889058896629663 ) ) ;
#5347 =( BOUNDED_CURVE ( )  B_SPLINE_CURVE ( 2, ( #6037, #8591, #9252, #8419, #801, #6754, #9585, #8816, #1935 ),
 .UNSPECIFIED., .F., .F. ) 
 B_SPLINE_CURVE_WITH_KNOTS ( ( 3, 2, 2, 2, 3 ),
 ( 0.4722222222222222099, 0.4814814814814814548, 0.5000000000000000000, 0.5185185185185184897, 0.5277777777777777901 ),
 .UNSPECIFIED. ) 
 CURVE ( )  GEOMETRIC_REPRESENTATION_ITEM ( )  RATIONAL_B_SPLINE_CURVE ( ( 0.9330127018922194093, 0.9330127018922194093, 1.000000000000000000, 0.8660254037844387076, 1.000000000000000000, 0.8660254037844387076, 1.000000000000000000, 0.9330127018922194093, 0.9330127018922194093 ) ) 
 REPRESENTATION_ITEM ( '' )  );
#5348 = ADVANCED_FACE ( 'NONE', ( #2074 ), #1755, .T. ) ;
#5349 = CARTESIAN_POINT ( 'NONE',  ( 23.22881793621964874, 18.67973499377871960, 11.95042449705234588 ) ) ;
#5350 = CARTESIAN_POINT ( 'NONE',  ( 20.08745147943499987, 17.71083118005251933, 12.00579112326941988 ) ) ;
#5351 = CARTESIAN_POINT ( 'NONE',  ( -25.17020516978313083, 53.80208333237728624, -3.596074190997380349 ) ) ;
#5352 = VECTOR ( 'NONE', #5902, 1000.000000000000000 ) ;
#5353 = DIRECTION ( 'NONE',  ( 0.000000000000000000, 0.000000000000000000, 1.000000000000000000 ) ) ;
#5354 = LINE ( 'NONE', #231, #4174 ) ;
#5355 = CARTESIAN_POINT ( 'NONE',  ( -25.98076211353311393, 49.49999999999986500, -5.000000000000103029 ) ) ;
#5356 = VERTEX_POINT ( 'NONE', #7855 ) ;
#5357 = EDGE_CURVE ( 'NONE', #3529, #2609, #2970, .T. ) ;
#5358 = CARTESIAN_POINT ( 'NONE',  ( 17.36588923991300604, 17.58385822839129986, 12.10347664333366247 ) ) ;
#5359 = AXIS2_PLACEMENT_3D ( 'NONE', #6988, #2777, #6150 ) ;
#5360 = CARTESIAN_POINT ( 'NONE',  ( 0.000000000000000000, 30.00000000000000000, -2.499999999999998668 ) ) ;
#5361 = CARTESIAN_POINT ( 'NONE',  ( 6.673314278414740999E-15, -2.686816014504674222, -2.346298152288229577 ) ) ;
#5362 = DIRECTION ( 'NONE',  ( 0.000000000000000000, 1.000000000000000000, 0.000000000000000000 ) ) ;
#5363 = CARTESIAN_POINT ( 'NONE',  ( 2.742827927723449299, 3.035229711104609596, -3.433252694550591233 ) ) ;
#5364 = DIRECTION ( 'NONE',  ( -1.000000000000000000, 0.000000000000000000, 0.000000000000000000 ) ) ;
#5365 = SURFACE_STYLE_USAGE ( .BOTH. , #10256 ) ;
#5366 = CARTESIAN_POINT ( 'NONE',  ( -1.449747468305836229, 33.50000000000000000, 13.73437500000000533 ) ) ;
#5367 = DIRECTION ( 'NONE',  ( -1.000000000000000000, -0.000000000000000000, -0.000000000000000000 ) ) ;
#5368 = ORIENTED_EDGE ( 'NONE', *, *, #9673, .T. ) ;
#5369 = CARTESIAN_POINT ( 'NONE',  ( 2.000000000000000000, -0.8865213383406730374, -1.535499999999999421 ) ) ;
#5370 = CARTESIAN_POINT ( 'NONE',  ( -2.500000000000007550, 31.03553390593274486, 16.39062500000000355 ) ) ;
#5371 = CARTESIAN_POINT ( 'NONE',  ( 2.500000000000010214, 28.96446609406726225, 14.51562500000000355 ) ) ;
#5372 = AXIS2_PLACEMENT_3D ( 'NONE', #10543, #10437, #9764 ) ;
#5373 = CYLINDRICAL_SURFACE ( 'NONE', #5237, 2.500000000000000444 ) ;
#5374 = CARTESIAN_POINT ( 'NONE',  ( 0.1388410611046027587, 2.351840044243008965, -2.926493552096035788 ) ) ;
#5375 = CARTESIAN_POINT ( 'NONE',  ( -24.35964822603314772, 53.45208333237727771, -5.935950539335252074 ) ) ;
#5376 = DIRECTION ( 'NONE',  ( 0.000000000000000000, 0.4999999999999993339, -0.8660254037844390407 ) ) ;
#5377 = CARTESIAN_POINT ( 'NONE',  ( -26.98076211353309972, 54.63333333333319786, -6.732050807568954909 ) ) ;
#5378 = CIRCLE ( 'NONE', #4123, 2.041999999999999815 ) ;
#5379 = ORIENTED_EDGE ( 'NONE', *, *, #892, .F. ) ;
#5380 = EDGE_CURVE ( 'NONE', #5275, #647, #2648, .T. ) ;
#5381 = ORIENTED_EDGE ( 'NONE', *, *, #6748, .T. ) ;
#5382 = DIRECTION ( 'NONE',  ( 0.000000000000000000, 0.000000000000000000, 1.000000000000000000 ) ) ;
#5383 = DIRECTION ( 'NONE',  ( -0.000000000000000000, 0.8660254037844431485, 0.4999999999999923395 ) ) ;
#5384 = ORIENTED_EDGE ( 'NONE', *, *, #8857, .F. ) ;
#5385 = CARTESIAN_POINT ( 'NONE',  ( 24.49999999999999289, 0.5000000000000132117, -4.999999999999992006 ) ) ;
#5386 = DIRECTION ( 'NONE',  ( 1.000000000000000000, 6.098637220230963674E-17, 1.156482317317871725E-16 ) ) ;
#5387 = EDGE_CURVE ( 'NONE', #7883, #3122, #8901, .T. ) ;
#5388 = CARTESIAN_POINT ( 'NONE',  ( 23.28338686706186778, 20.94194386221399640, 11.00732503135556861 ) ) ;
#5389 = ORIENTED_EDGE ( 'NONE', *, *, #5876, .F. ) ;
#5390 = EDGE_CURVE ( 'NONE', #3024, #6057, #7018, .T. ) ;
#5391 = CARTESIAN_POINT ( 'NONE',  ( -26.79131905728310059, 52.46041666571061768, -3.596074190997381237 ) ) ;
#5392 = LINE ( 'NONE', #1052, #8743 ) ;
#5393 = ORIENTED_EDGE ( 'NONE', *, *, #9877, .F. ) ;
#5394 = CARTESIAN_POINT ( 'NONE',  ( 29.50000000000000711, 2.000000000000001776, 15.49999999999999645 ) ) ;
#5395 = ORIENTED_EDGE ( 'NONE', *, *, #1972, .T. ) ;
#5396 = CARTESIAN_POINT ( 'NONE',  ( -1.720978244806803170, 28.18544433887405987, 14.37719158473306713 ) ) ;
#5397 = ORIENTED_EDGE ( 'NONE', *, *, #2625, .T. ) ;
#5398 = CARTESIAN_POINT ( 'NONE',  ( 21.82671760412675610, 17.70440453107251244, 11.95042449705224819 ) ) ;
#5399 = PRESENTATION_STYLE_ASSIGNMENT (( #8058 ) ) ;
#5400 = EDGE_CURVE ( 'NONE', #6302, #8576, #471, .T. ) ;
#5401 = CIRCLE ( 'NONE', #4693, 2.500000000000000888 ) ;
#5402 = CARTESIAN_POINT ( 'NONE',  ( 23.89484671925281845, 19.39402032390267649, 11.95042449705224819 ) ) ;
#5403 = ADVANCED_FACE ( 'NONE', ( #288 ), #4208, .T. ) ;
#5404 = CARTESIAN_POINT ( 'NONE',  ( 21.28817020210873423, 18.47861593500339694, 13.00425721518307576 ) ) ;
#5405 = CARTESIAN_POINT ( 'NONE',  ( -27.60187600103308014, 53.51041666571062194, -5.935950539335252074 ) ) ;
#5406 = LINE ( 'NONE', #7124, #1217 ) ;
#5407 = CARTESIAN_POINT ( 'NONE',  ( 26.25045812061784289, 56.49999999999984368, 10.00000000000000178 ) ) ;
#5408 = CARTESIAN_POINT ( 'NONE',  ( -24.98076211353313170, 52.79583333142137036, -3.267949192431250705 ) ) ;
#5409 = VERTEX_POINT ( 'NONE', #1331 ) ;
#5410 =( BOUNDED_CURVE ( )  B_SPLINE_CURVE ( 2, ( #1326, #3776, #4668, #325, #3828, #9826, #7214, #4618, #2163, #3053, #3721, #10505, #2895, #3882, #6264, #10607, #9658, #2054, #2212, #7266, #8003, #5610, #3005, #6383, #8935, #4727, #8104, #482, #8993, #1383, #3151, #643, #3200, #6637, #533, #1650, #5872, #1539, #8157, #4879, #6580, #5817, #7373, #10816, #4941, #8259, #4039, #9982, #7426, #10101, #9255, #6702, #2367, #1482, #5760, #3932, #8204, #6535, #2487, #2428, #4829, #10759, #9143, #9932, #8313, #9879, #7316, #2317, #695, #4093, #7481, #10869, #5708, #3258, #9088, #10042, #9202, #1595, #584, #10705, #4992, #2270, #8366, #745, #4145, #7537, #10926, #3100, #3318, #6479, #5662, #9041, #1432, #3979, #9538, #32, #5217, #868, #8594, #7656, #10987, #9481, #1879, #8484, #5047 ),
 .UNSPECIFIED., .F., .F. ) 
 B_SPLINE_CURVE_WITH_KNOTS ( ( 3, 2, 2, 2, 2, 2, 2, 2, 2, 2, 2, 2, 2, 2, 2, 2, 2, 2, 2, 2, 2, 2, 2, 2, 2, 2, 2, 2, 2, 2, 2, 2, 2, 2, 2, 2, 2, 2, 2, 2, 2, 2, 2, 2, 2, 2, 2, 2, 2, 2, 2, 2, 3 ),
 ( 0.000000000000000000, 0.01851851851851851749, 0.03703703703703703498, 0.05555555555555555247, 0.07407407407407406996, 0.09259259259259258745, 0.1111111111111111049, 0.1296296296296296224, 0.1481481481481481399, 0.1666666666666666574, 0.1851851851851851749, 0.2037037037037036924, 0.2222222222222222099, 0.2407407407407407274, 0.2592592592592592449, 0.2777777777777777901, 0.2962962962962962798, 0.3148148148148148806, 0.3333333333333333148, 0.3518518518518518601, 0.3703703703703703498, 0.3888888888888888951, 0.4074074074074073848, 0.4259259259259259300, 0.4444444444444444198, 0.4629629629629629650, 0.4814814814814814548, 0.5000000000000000000, 0.5185185185185184897, 0.5370370370370370905, 0.5555555555555555802, 0.5740740740740740700, 0.5925925925925925597, 0.6111111111111111605, 0.6296296296296297612, 0.6481481481481481399, 0.6666666666666666297, 0.6851851851851852304, 0.7037037037037037202, 0.7222222222222222099, 0.7407407407407406996, 0.7592592592592594114, 0.7777777777777777901, 0.7962962962962962798, 0.8148148148148147696, 0.8333333333333333703, 0.8518518518518518601, 0.8703703703703703498, 0.8888888888888888395, 0.9074074074074074403, 0.9259259259259259300, 0.9444444444444444198, 0.9524110019551521589 ),
 .UNSPECIFIED. ) 
 CURVE ( )  GEOMETRIC_REPRESENTATION_ITEM ( )  RATIONAL_B_SPLINE_CURVE ( ( 1.000000000000000000, 0.8660254037844387076, 1.000000000000000000, 0.8660254037844387076, 1.000000000000000000, 0.8660254037844387076, 1.000000000000000000, 0.8660254037844387076, 1.000000000000000000, 0.8660254037844387076, 1.000000000000000000, 0.8660254037844387076, 1.000000000000000000, 0.8660254037844387076, 1.000000000000000000, 0.8660254037844387076, 1.000000000000000000, 0.8660254037844387076, 1.000000000000000000, 0.8660254037844387076, 1.000000000000000000, 0.8660254037844387076, 1.000000000000000000, 0.8660254037844387076, 1.000000000000000000, 0.8660254037844387076, 1.000000000000000000, 0.8660254037844387076, 1.000000000000000000, 0.8660254037844387076, 1.000000000000000000, 0.8660254037844387076, 1.000000000000000000, 0.8660254037844387076, 1.000000000000000000, 0.8660254037844387076, 1.000000000000000000, 0.8660254037844387076, 1.000000000000000000, 0.8660254037844387076, 1.000000000000000000, 0.8660254037844387076, 1.000000000000000000, 0.8660254037844387076, 1.000000000000000000, 0.8660254037844387076, 1.000000000000000000, 0.8660254037844387076, 1.000000000000000000, 0.8660254037844387076, 1.000000000000000000, 0.8660254037844387076, 1.000000000000000000, 0.8660254037844387076, 1.000000000000000000, 0.8660254037844387076, 1.000000000000000000, 0.8660254037844387076, 1.000000000000000000, 0.8660254037844387076, 1.000000000000000000, 0.8660254037844387076, 1.000000000000000000, 0.8660254037844387076, 1.000000000000000000, 0.8660254037844387076, 1.000000000000000000, 0.8660254037844387076, 1.000000000000000000, 0.8660254037844387076, 1.000000000000000000, 0.8660254037844387076, 1.000000000000000000, 0.8660254037844387076, 1.000000000000000000, 0.8660254037844387076, 1.000000000000000000, 0.8660254037844387076, 1.000000000000000000, 0.8660254037844387076, 1.000000000000000000, 0.8660254037844387076, 1.000000000000000000, 0.8660254037844387076, 1.000000000000000000, 0.8660254037844387076, 1.000000000000000000, 0.8660254037844387076, 1.000000000000000000, 0.8660254037844387076, 1.000000000000000000, 0.8660254037844387076, 1.000000000000000000, 0.8660254037844387076, 1.000000000000000000, 0.8660254037844387076, 1.000000000000000000, 0.8660254037844387076, 1.000000000000000000, 0.8660254037844387076, 1.000000000000000000, 0.8660254037844387076, 1.000000000000000000, 0.9423649184108428001, 0.9343183815700366601 ) ) 
 REPRESENTATION_ITEM ( '' )  );
#5411 = VECTOR ( 'NONE', #9266, 1000.000000000000114 ) ;
#5412 = CARTESIAN_POINT ( 'NONE',  ( 2.000000000000000000, -0.8865213383406694847, 1.535500000000001419 ) ) ;
#5413 = CARTESIAN_POINT ( 'NONE',  ( 3.199999999999999734, 3.031088913245550742, 1.749999999999972466 ) ) ;
#5414 = CARTESIAN_POINT ( 'NONE',  ( 0.2500000000000002220, 0.000000000000000000, 4.000000000000000000 ) ) ;
#5415 = CIRCLE ( 'NONE', #3646, 3.000000000000000888 ) ;
#5416 = DIRECTION ( 'NONE',  ( 1.000000000000000000, 0.000000000000000000, 0.000000000000000000 ) ) ;
#5417 = DIRECTION ( 'NONE',  ( 1.000000000000000000, 0.000000000000000000, 0.000000000000000000 ) ) ;
#5418 = CARTESIAN_POINT ( 'NONE',  ( -26.51666049839535333, 52.70623925897106687, -3.000000000000132339 ) ) ;
#5419 = DIRECTION ( 'NONE',  ( 0.000000000000000000, 0.000000000000000000, -1.000000000000000000 ) ) ;
#5420 = AXIS2_PLACEMENT_3D ( 'NONE', #1025, #10981, #4262 ) ;
#5421 =( NAMED_UNIT ( * ) SI_UNIT ( $, .STERADIAN. ) SOLID_ANGLE_UNIT ( ) );
#5422 = CARTESIAN_POINT ( 'NONE',  ( -1.734723475976807094E-15, 33.50000000000000000, 14.90625000000000355 ) ) ;
#5423 = DIRECTION ( 'NONE',  ( 0.000000000000000000, -1.000000000000000000, 0.000000000000000000 ) ) ;
#5424 = EDGE_LOOP ( 'NONE', ( #5111, #2472 ) ) ;
#5425 = LINE ( 'NONE', #4703, #3320 ) ;
#5426 = VECTOR ( 'NONE', #6414, 1000.000000000000000 ) ;
#5427 = CARTESIAN_POINT ( 'NONE',  ( 1.814555661125939467, 31.72097824480680828, 15.74780841526694175 ) ) ;
#5428 = CARTESIAN_POINT ( 'NONE',  ( 2.500000000000008438, 30.00000000000000711, 14.59375000000000178 ) ) ;
#5429 = VECTOR ( 'NONE', #2247, 1000.000000000000000 ) ;
#5430 = CARTESIAN_POINT ( 'NONE',  ( 23.33980466280999977, 20.94445964013513617, 12.00579112326902909 ) ) ;
#5431 = CARTESIAN_POINT ( 'NONE',  ( -26.59870219654672141, 57.20337143919491041, -6.904607032842216441 ) ) ;
#5432 = CARTESIAN_POINT ( 'NONE',  ( 4.000000000000003553, 0.000000000000000000, 0.000000000000000000 ) ) ;
#5433 = AXIS2_PLACEMENT_3D ( 'NONE', #8697, #6132, #8803 ) ;
#5434 = CARTESIAN_POINT ( 'NONE',  ( -3.455068668934486276, 2.624017327439035707, -3.316620875263955437 ) ) ;
#5435 = CARTESIAN_POINT ( 'NONE',  ( -24.35964822603314772, 51.23541666571061626, -4.064049460664953983 ) ) ;
#5436 = LINE ( 'NONE', #8760, #7856 ) ;
#5437 = CIRCLE ( 'NONE', #628, 4.500000000000000000 ) ;
#5438 = ORIENTED_EDGE ( 'NONE', *, *, #6361, .T. ) ;
#5439 = ORIENTED_EDGE ( 'NONE', *, *, #6409, .F. ) ;
#5440 = LINE ( 'NONE', #1094, #1314 ) ;
#5441 = CARTESIAN_POINT ( 'NONE',  ( -25.98076211353311393, 49.49999999999986500, -7.000000000000074607 ) ) ;
#5442 = ITEM_DEFINED_TRANSFORMATION ( 'NONE', 'NONE', #4206,  #308 ) ;
#5443 = ORIENTED_EDGE ( 'NONE', *, *, #1449, .F. ) ;
#5444 = LINE ( 'NONE', #10503, #10028 ) ;
#5445 = AXIS2_PLACEMENT_3D ( 'NONE', #1138, #1199, #9702 ) ;
#5446 = CARTESIAN_POINT ( 'NONE',  ( 3.333333333333332593, 2.694301256218250007, -3.300726591567078483 ) ) ;
#5447 = CARTESIAN_POINT ( 'NONE',  ( 24.26768760078471487, 20.42249838054411271, 10.95195840513859586 ) ) ;
#5448 = ORIENTED_EDGE ( 'NONE', *, *, #7524, .T. ) ;
#5449 = CARTESIAN_POINT ( 'NONE',  ( -24.35964822603314772, 54.03541666571061342, -4.064049460664953983 ) ) ;
#5450 = ORIENTED_EDGE ( 'NONE', *, *, #6135, .F. ) ;
#5451 = DIRECTION ( 'NONE',  ( -6.098637220230963674E-17, 1.000000000000000000, 0.000000000000000000 ) ) ;
#5452 = ORIENTED_EDGE ( 'NONE', *, *, #8466, .T. ) ;
#5453 = B_SPLINE_CURVE_WITH_KNOTS ( 'NONE', 3,
 ( #7289, #8964, #3856, #1187, #7241, #10731 ),
 .UNSPECIFIED., .F., .F.,
 ( 4, 2, 4 ),
 ( 0.005702039456357537589, 0.006725091618211279793, 0.007748143780065021996 ),
 .UNSPECIFIED. ) ;
#5454 = CARTESIAN_POINT ( 'NONE',  ( 0.9693646802875628410, 32.52740819067395961, 15.08031658473306891 ) ) ;
#5455 = ORIENTED_EDGE ( 'NONE', *, *, #1537, .F. ) ;
#5456 = CARTESIAN_POINT ( 'NONE',  ( 17.34774915531493278, 16.33073436721105054, 11.04457336562047765 ) ) ;
#5457 = AXIS2_PLACEMENT_3D ( 'NONE', #10329, #6212, #8605 ) ;
#5458 = DIRECTION ( 'NONE',  ( 1.000000000000000000, 0.000000000000000000, 0.000000000000000000 ) ) ;
#5459 = CARTESIAN_POINT ( 'NONE',  ( 19.78966864679935611, 21.38900865752197689, 13.00425721518248956 ) ) ;
#5460 = CARTESIAN_POINT ( 'NONE',  ( -24.98076211353312814, 49.61666666666653214, -6.732050807568954909 ) ) ;
#5461 = DIRECTION ( 'NONE',  ( -1.000000000000000000, -6.098637220230963674E-17, -1.156482317317871478E-16 ) ) ;
#5462 = AXIS2_PLACEMENT_3D ( 'NONE', #7693, #10132, #127 ) ;
#5463 = AXIS2_PLACEMENT_3D ( 'NONE', #5516, #6439, #4684 ) ;
#5464 = DIRECTION ( 'NONE',  ( 0.000000000000000000, 0.000000000000000000, 1.000000000000000000 ) ) ;
#5465 = CARTESIAN_POINT ( 'NONE',  ( 1.567478505476134606E-15, 4.618802153517012066, -5.000000000000000000 ) ) ;
#5466 = ORIENTED_EDGE ( 'NONE', *, *, #8112, .T. ) ;
#5467 = EDGE_CURVE ( 'NONE', #8941, #5409, #10447, .T. ) ;
#5468 = ORIENTED_EDGE ( 'NONE', *, *, #4517, .T. ) ;
#5469 = EDGE_CURVE ( 'NONE', #4079, #3081, #3874, .T. ) ;
#5470 = CARTESIAN_POINT ( 'NONE',  ( 17.64011212484924940, 17.30965061758477219, 13.07995645546588825 ) ) ;
#5471 = CARTESIAN_POINT ( 'NONE',  ( 24.49999999999998934, -1.232050807568860762, 10.00000000000000888 ) ) ;
#5472 = PRODUCT_DEFINITION_SHAPE ( 'NONE', 'NONE',  #11005 ) ;
#5473 = VECTOR ( 'NONE', #5234, 1000.000000000000000 ) ;
#5474 = FILL_AREA_STYLE ('',( #10472 ) ) ;
#5475 = CARTESIAN_POINT ( 'NONE',  ( -26.11341725377009482, 59.00000000000061107, -3.000000000000243805 ) ) ;
#5476 =( GEOMETRIC_REPRESENTATION_CONTEXT ( 3 ) GLOBAL_UNCERTAINTY_ASSIGNED_CONTEXT ( ( #8083 ) ) GLOBAL_UNIT_ASSIGNED_CONTEXT ( ( #4537, #6976, #5421 ) ) REPRESENTATION_CONTEXT ( 'NONE', 'WORKASPACE' ) );
#5477 = DIRECTION ( 'NONE',  ( -0.000000000000000000, 1.000000000000000000, -0.000000000000000000 ) ) ;
#5478 = CARTESIAN_POINT ( 'NONE',  ( 29.49999999999999645, -3.999999999999986233, -4.999999999999991118 ) ) ;
#5479 =( LENGTH_UNIT ( ) NAMED_UNIT ( * ) SI_UNIT ( .MILLI., .METRE. ) );
#5480 = CARTESIAN_POINT ( 'NONE',  ( -21.21106610644865498, 13.49999999999941913, -9.500000000000000000 ) ) ;
#5481 = CARTESIAN_POINT ( 'NONE',  ( -3.500000000000003109, 29.99999999999999645, 13.96875000000000355 ) ) ;
#5482 = CARTESIAN_POINT ( 'NONE',  ( -3.511755186886750479, 2.826662030176366081, -3.597382984111578086 ) ) ;
#5483 = ORIENTED_EDGE ( 'NONE', *, *, #1769, .T. ) ;
#5484 = CARTESIAN_POINT ( 'NONE',  ( 0.000000000000000000, 0.000000000000000000, 0.000000000000000000 ) ) ;
#5485 = AXIS2_PLACEMENT_3D ( 'NONE', #7174, #4686, #8688 ) ;
#5486 = EDGE_CURVE ( 'NONE', #6952, #10021, #6694, .T. ) ;
#5487 = CARTESIAN_POINT ( 'NONE',  ( -2.428085025993355295, 32.52166244231248271, 14.81030841526694175 ) ) ;
#5488 = VECTOR ( 'NONE', #9747, 1000.000000000000000 ) ;
#5489 = DIRECTION ( 'NONE',  ( -0.1561119869140000782, 0.9855205127846302648, -0.06616922564517753458 ) ) ;
#5490 = DIRECTION ( 'NONE',  ( 1.000000000000000000, 0.000000000000000000, 0.000000000000000000 ) ) ;
#5491 = CARTESIAN_POINT ( 'NONE',  ( -25.98076211353311393, 54.83749999808802755, -3.000000000000132339 ) ) ;
#5492 = PLANE ( 'NONE',  #7726 ) ;
#5493 = EDGE_CURVE ( 'NONE', #7488, #8716, #1280, .T. ) ;
#5494 = CARTESIAN_POINT ( 'NONE',  ( -4.175648173966055587, 2.207990556236529844, -3.469390959564062626 ) ) ;
#5495 = CARTESIAN_POINT ( 'NONE',  ( -27.60187600103308014, 51.70208333237727771, -4.064049460664955760 ) ) ;
#5496 = DIRECTION ( 'NONE',  ( 1.000000000000000000, 6.098637220230963674E-17, 0.000000000000000000 ) ) ;
#5497 = CARTESIAN_POINT ( 'NONE',  ( 34.64101615137754209, 5.000000000000001776, -2.500000000000000000 ) ) ;
#5498 = ORIENTED_EDGE ( 'NONE', *, *, #8266, .T. ) ;
#5499 = DIRECTION ( 'NONE',  ( 0.000000000000000000, 1.000000000000000000, 0.000000000000000000 ) ) ;
#5500 = LINE ( 'NONE', #10444, #7528 ) ;
#5501 = ORIENTED_EDGE ( 'NONE', *, *, #7851, .T. ) ;
#5502 = EDGE_CURVE ( 'NONE', #702, #1959, #9210, .T. ) ;
#5503 = DIRECTION ( 'NONE',  ( 0.000000000000000000, 0.000000000000000000, 1.000000000000000000 ) ) ;
#5504 = LINE ( 'NONE', #1277, #267 ) ;
#5505 = CARTESIAN_POINT ( 'NONE',  ( 19.82941471729559524, 23.00258574805652856, 10.95195840513859231 ) ) ;
#5506 = ORIENTED_EDGE ( 'NONE', *, *, #305, .T. ) ;
#5507 = CARTESIAN_POINT ( 'NONE',  ( -27.60187600103308370, 51.64374999904394770, -5.000000000000103029 ) ) ;
#5508 = ORIENTED_EDGE ( 'NONE', *, *, #10570, .T. ) ;
#5509 = CARTESIAN_POINT ( 'NONE',  ( 1.047444401652940007E-13, 30.00000000000000000, 2.500000000000000000 ) ) ;
#5510 = ORIENTED_EDGE ( 'NONE', *, *, #10557, .F. ) ;
#5511 = CARTESIAN_POINT ( 'NONE',  ( 1.035533905932737975, 32.50000000000000711, 14.82812500000000178 ) ) ;
#5512 = FILL_AREA_STYLE_COLOUR ( '', #1367 ) ;
#5513 = EDGE_LOOP ( 'NONE', ( #2284, #6652, #1226, #3360 ) ) ;
#5514 = CARTESIAN_POINT ( 'NONE',  ( 15.59693448110033032, 17.93859942483392800, 11.20086348037537327 ) ) ;
#5515 = APPLICATION_CONTEXT ( 'automotive_design' ) ;
#5516 = CARTESIAN_POINT ( 'NONE',  ( 34.99999999999987210, -3.999999999999989786, -4.999999999999999112 ) ) ;
#5517 = CARTESIAN_POINT ( 'NONE',  ( 21.41520517525563605, 22.70178780811528441, 13.00425721518307753 ) ) ;
#5518 = CARTESIAN_POINT ( 'NONE',  ( 2.550604951803072673, 0.000000000000000000, 0.000000000000000000 ) ) ;
#5519 = CARTESIAN_POINT ( 'NONE',  ( 5.560781378645573980, 6.809993116116507654E-16, -4.000000000000000000 ) ) ;
#5520 = CARTESIAN_POINT ( 'NONE',  ( 24.55500000000002103, 0.000000000000000000, 0.000000000000000000 ) ) ;
#5521 = ADVANCED_FACE ( 'NONE', ( #4783 ), #10613, .T. ) ;
#5522 = ORIENTED_EDGE ( 'NONE', *, *, #7228, .F. ) ;
#5523 = VERTEX_POINT ( 'NONE', #3886 ) ;
#5524 = CARTESIAN_POINT ( 'NONE',  ( 20.43380676890320657, 22.25420293214091316, 12.00579112326941988 ) ) ;
#5525 = CARTESIAN_POINT ( 'NONE',  ( 1.047444401652940007E-13, 30.00000000000000000, -2.500000000000000000 ) ) ;
#5526 = DIRECTION ( 'NONE',  ( 0.000000000000000000, 0.000000000000000000, 1.000000000000000000 ) ) ;
#5527 = CIRCLE ( 'NONE', #373, 7.500000000000000000 ) ;
#5528 = CARTESIAN_POINT ( 'NONE',  ( 4.000000000000000000, -2.309401076758514915, -3.433295621305383349 ) ) ;
#5529 = DIRECTION ( 'NONE',  ( -1.000000000000000000, 0.000000000000000000, 0.000000000000000000 ) ) ;
#5530 = EDGE_CURVE ( 'NONE', #7117, #3819, #1394, .T. ) ;
#5531 = SURFACE_SIDE_STYLE ('',( #3911 ) ) ;
#5532 = CARTESIAN_POINT ( 'NONE',  ( 0.06616922564517314920, 33.50000000000000000, 17.15405841526694175 ) ) ;
#5533 = LINE ( 'NONE', #1466, #104 ) ;
#5534 = EDGE_LOOP ( 'NONE', ( #10246, #4895, #2313, #8374 ) ) ;
#5535 =( LENGTH_UNIT ( ) NAMED_UNIT ( * ) SI_UNIT ( .MILLI., .METRE. ) );
#5536 = EDGE_CURVE ( 'NONE', #433, #3324, #9525, .T. ) ;
#5537 = AXIS2_PLACEMENT_3D ( 'NONE', #9067, #10794, #1514 ) ;
#5538 = CARTESIAN_POINT ( 'NONE',  ( 3.472591809326051937, 28.48408330604899419, 15.51343341526694353 ) ) ;
#5539 = DIRECTION ( 'NONE',  ( -0.7071067811865292541, 8.659560562355155958E-17, -0.7071067811865657804 ) ) ;
#5540 = LINE ( 'NONE', #7880, #5253 ) ;
#5541 = MANIFOLD_SOLID_BREP ( 'Fillet4', #10725 ) ;
#5542 = EDGE_CURVE ( 'NONE', #6762, #7090, #1933, .T. ) ;
#5543 = CARTESIAN_POINT ( 'NONE',  ( -25.98076211353311393, 51.42499999999986926, -3.000000000000132339 ) ) ;
#5544 = CARTESIAN_POINT ( 'NONE',  ( -25.17020516978313083, 51.17708333237727913, -3.596074190997380349 ) ) ;
#5545 = CARTESIAN_POINT ( 'NONE',  ( 24.49999999999999289, -6.767949192431106376, 10.00000000000001243 ) ) ;
#5546 = CARTESIAN_POINT ( 'NONE',  ( -3.453038570459499024, -2.625189405340453419, -3.535263753545272891 ) ) ;
#5547 = EDGE_LOOP ( 'NONE', ( #2217, #8490, #10967 ) ) ;
#5548 = AXIS2_PLACEMENT_3D ( 'NONE', #4270, #1037, #8487 ) ;
#5549 = DIRECTION ( 'NONE',  ( -0.000000000000000000, -0.000000000000000000, 1.000000000000000000 ) ) ;
#5550 = EDGE_CURVE ( 'NONE', #1351, #5059, #3544, .T. ) ;
#5551 = EDGE_CURVE ( 'NONE', #3326, #10134, #3339, .T. ) ;
#5552 = ORIENTED_EDGE ( 'NONE', *, *, #5551, .F. ) ;
#5553 = CARTESIAN_POINT ( 'NONE',  ( -25.98076211353311393, 49.49999999999986500, -5.000000000000103029 ) ) ;
#5554 = CARTESIAN_POINT ( 'NONE',  ( -25.98076211353311038, 61.49999999999985789, -8.500000000000694556 ) ) ;
#5555 = VECTOR ( 'NONE', #4462, 1000.000000000000114 ) ;
#5556 = CARTESIAN_POINT ( 'NONE',  ( 18.58376669197321007, 17.02366754649298031, 11.02344032946268548 ) ) ;
#5557 = ORIENTED_EDGE ( 'NONE', *, *, #6626, .T. ) ;
#5558 = CARTESIAN_POINT ( 'NONE',  ( 5.200000000000002842, 3.306546357697854719E-16, 2.700000000000001066 ) ) ;
#5559 = MANIFOLD_SOLID_BREP ( 'Fillet4', #3273 ) ;
#5560 = ORIENTED_EDGE ( 'NONE', *, *, #5550, .T. ) ;
#5561 = FACE_OUTER_BOUND ( 'NONE', #507, .T. ) ;
#5562 = VERTEX_POINT ( 'NONE', #2660 ) ;
#5563 = CARTESIAN_POINT ( 'NONE',  ( 2.527408190673965382, 29.03063531971243449, 14.76781658473306535 ) ) ;
#5564 = FILL_AREA_STYLE ('',( #5512 ) ) ;
#5565 = ORIENTED_EDGE ( 'NONE', *, *, #7649, .F. ) ;
#5566 = CARTESIAN_POINT ( 'NONE',  ( 16.06885556321644160, 18.88089190506775594, 11.22291988893967840 ) ) ;
#5567 =( LENGTH_UNIT ( ) NAMED_UNIT ( * ) SI_UNIT ( .MILLI., .METRE. ) );
#5568 = ADVANCED_FACE ( 'NONE', ( #6927 ), #10315, .F. ) ;
#5569 = ADVANCED_FACE ( 'NONE', ( #194 ), #7248, .F. ) ;
#5570 = CARTESIAN_POINT ( 'NONE',  ( -0.02448733951239248641, -4.877042772274742255, -3.751161874094027571 ) ) ;
#5571 = CARTESIAN_POINT ( 'NONE',  ( 16.08167231043895384, 17.45386159549338245, 13.15979613361243494 ) ) ;
#5572 = CARTESIAN_POINT ( 'NONE',  ( -23.98076211353314235, 52.85416666475470748, -3.845299461620867554 ) ) ;
#5573 = CARTESIAN_POINT ( 'NONE',  ( 34.92408131826248052, 2.305272916965853014, -4.166859826334558647 ) ) ;
#5574 = CARTESIAN_POINT ( 'NONE',  ( 2.887392608830370744, 2.020725942163657862, -3.499999999999999556 ) ) ;
#5575 = VERTEX_POINT ( 'NONE', #2824 ) ;
#5576 = ORIENTED_EDGE ( 'NONE', *, *, #9957, .T. ) ;
#5577 = CARTESIAN_POINT ( 'NONE',  ( 19.95755123817951215, 17.62047157401400810, 12.00579112326941988 ) ) ;
#5578 = MANIFOLD_SOLID_BREP ( 'EndChamfer', #7010 ) ;
#5579 = CIRCLE ( 'NONE', #762, 1.610000000000000098 ) ;
#5580 = DIRECTION ( 'NONE',  ( 1.000000000000000000, 0.000000000000000000, 0.000000000000000000 ) ) ;
#5581 = CARTESIAN_POINT ( 'NONE',  ( -26.98076211353309972, 49.96666666666652645, -3.267949192431252037 ) ) ;
#5582 = CARTESIAN_POINT ( 'NONE',  ( 24.49999999999999289, -3.999999999999986233, -4.999999999999992006 ) ) ;
#5583 = CARTESIAN_POINT ( 'NONE',  ( 2.521662442312485819, 32.42808502599335441, 16.99780841526693820 ) ) ;
#5584 = CARTESIAN_POINT ( 'NONE',  ( -2.805705207896067144, 3.226868319750155312, -3.503898532754364581 ) ) ;
#5585 = AXIS2_PLACEMENT_3D ( 'NONE', #7054, #2839, #6211 ) ;
#5586 = VERTEX_POINT ( 'NONE', #5369 ) ;
#5587 = CARTESIAN_POINT ( 'NONE',  ( 0.3126073911696448659, -4.041451884327390331, 2.328673539876467720E-14 ) ) ;
#5588 = CARTESIAN_POINT ( 'NONE',  ( -2.505208318772514708, 29.86938897312880314, 17.48140433884295319 ) ) ;
#5589 = AXIS2_PLACEMENT_3D ( 'NONE', #8203, #7536, #2269 ) ;
#5590 = PLANE ( 'NONE',  #7019 ) ;
#5591 = CARTESIAN_POINT ( 'NONE',  ( 2.500000000000000000, 0.000000000000000000, 0.000000000000000000 ) ) ;
#5592 = AXIS2_PLACEMENT_3D ( 'NONE', #8102, #480, #3930 ) ;
#5593 = CARTESIAN_POINT ( 'NONE',  ( 3.200000000000000178, 2.020725942163738686, 3.499999999999999556 ) ) ;
#5594 = CARTESIAN_POINT ( 'NONE',  ( -0.5469614295416921346, 4.303013824936271270, -3.535263753543735454 ) ) ;
#5595 = CARTESIAN_POINT ( 'NONE',  ( -27.60187600103308014, 53.80208333237727203, -4.064049460664955760 ) ) ;
#5596 = CARTESIAN_POINT ( 'NONE',  ( 1.393927851585479161, -4.043713361053543842, -3.526374918436840922 ) ) ;
#5597 = CARTESIAN_POINT ( 'NONE',  ( -1.287237434361707233, -3.875615274277397937, -3.430618716626816500 ) ) ;
#5598 = AXIS2_PLACEMENT_3D ( 'NONE', #707, #3166, #10833 ) ;
#5599 = VERTEX_POINT ( 'NONE', #7139 ) ;
#5600 = VECTOR ( 'NONE', #10676, 1000.000000000000000 ) ;
#5601 = AXIS2_PLACEMENT_3D ( 'NONE', #3917, #7354, #8192 ) ;
#5602 = VECTOR ( 'NONE', #10876, 1000.000000000000000 ) ;
#5603 = CARTESIAN_POINT ( 'NONE',  ( -1.654252653721913102, -3.663718938583024443, -0.01223254789874440342 ) ) ;
#5604 = ADVANCED_FACE ( 'NONE', ( #7195, #9754, #1255 ), #10931, .T. ) ;
#5605 = ITEM_DEFINED_TRANSFORMATION ( 'NONE', 'NONE', #8650,  #308 ) ;
#5606 = VERTEX_POINT ( 'NONE', #10646 ) ;
#5607 = EDGE_CURVE ( 'NONE', #8525, #7309, #2930, .T. ) ;
#5608 = CARTESIAN_POINT ( 'NONE',  ( -4.000000000000000000, 2.309401076758498483, -3.433295621305379353 ) ) ;
#5609 = AXIS2_PLACEMENT_3D ( 'NONE', #5634, #10637, #5580 ) ;
#5610 = CARTESIAN_POINT ( 'NONE',  ( -25.98076211353310683, 50.94374999904394485, -3.128098921329806714 ) ) ;
#5611 = VECTOR ( 'NONE', #9082, 1000.000000000000000 ) ;
#5612 = CARTESIAN_POINT ( 'NONE',  ( 20.05551109708751412, 20.00475302350064766, 11.00732503135517426 ) ) ;
#5613 = EDGE_LOOP ( 'NONE', ( #7626, #10268, #2850, #8380 ) ) ;
#5614 = CARTESIAN_POINT ( 'NONE',  ( -26.98076211353309972, 53.84583333142136752, -6.732050807568954909 ) ) ;
#5615 = ORIENTED_EDGE ( 'NONE', *, *, #693, .F. ) ;
#5616 = CARTESIAN_POINT ( 'NONE',  ( 0.2949799022107380542, 0.000000000000000000, 0.000000000000000000 ) ) ;
#5617 = ORIENTED_EDGE ( 'NONE', *, *, #3686, .T. ) ;
#5618 = FACE_OUTER_BOUND ( 'NONE', #8349, .T. ) ;
#5619 =( NAMED_UNIT ( * ) SI_UNIT ( $, .STERADIAN. ) SOLID_ANGLE_UNIT ( ) );
#5620 = AXIS2_PLACEMENT_3D ( 'NONE', #7753, #10356, #6025 ) ;
#5621 = ORIENTED_EDGE ( 'NONE', *, *, #4961, .T. ) ;
#5622 = CARTESIAN_POINT ( 'NONE',  ( 22.42093126068789033, 23.47289781856171587, 10.95195840513859231 ) ) ;
#5623 = DIRECTION ( 'NONE',  ( 1.000000000000000000, 6.098637220230963674E-17, -0.000000000000000000 ) ) ;
#5624 = CARTESIAN_POINT ( 'NONE',  ( 15.69051189741946573, 17.84502200851479614, 13.19648031090924789 ) ) ;
#5625 = VECTOR ( 'NONE', #3416, 1000.000000000000000 ) ;
#5626 = CARTESIAN_POINT ( 'NONE',  ( -24.98076211353312814, 50.92916666475470322, -6.732050807568954909 ) ) ;
#5627 = DIRECTION ( 'NONE',  ( 0.000000000000000000, 0.000000000000000000, -1.000000000000000000 ) ) ;
#5628 = DIRECTION ( 'NONE',  ( 0.000000000000000000, -0.000000000000000000, 1.000000000000000000 ) ) ;
#5629 = ORIENTED_EDGE ( 'NONE', *, *, #3962, .T. ) ;
#5630 = PRODUCT_DEFINITION_FORMATION_WITH_SPECIFIED_SOURCE ( 'ANY', '', #10340, .NOT_KNOWN. ) ;
#5631 = ORIENTED_EDGE ( 'NONE', *, *, #2477, .T. ) ;
#5632 = CARTESIAN_POINT ( 'NONE',  ( 21.41951502703731691, 22.64547864373410135, 12.00579112326941988 ) ) ;
#5633 = EDGE_CURVE ( 'NONE', #1334, #4847, #5425, .T. ) ;
#5634 = CARTESIAN_POINT ( 'NONE',  ( 0.000000000000000000, 0.000000000000000000, -5.000000000000000000 ) ) ;
#5635 = AXIS2_PLACEMENT_3D ( 'NONE', #4127, #9071, #8402 ) ;
#5636 = AXIS2_PLACEMENT_3D ( 'NONE', #2332, #7442, #8275 ) ;
#5637 = CARTESIAN_POINT ( 'NONE',  ( 0.6666666666666658525, -4.233901974057276085, -3.300726591567086476 ) ) ;
#5638 = DIRECTION ( 'NONE',  ( 0.000000000000000000, -0.4999999999999993894, 0.8660254037844389297 ) ) ;
#5639 = CARTESIAN_POINT ( 'NONE',  ( 0.000000000000000000, 0.000000000000000000, 2.500000000000000000 ) ) ;
#5640 = CARTESIAN_POINT ( 'NONE',  ( -1.101703131577916883, 32.47259180932605460, 12.73656658473306358 ) ) ;
#5641 = CARTESIAN_POINT ( 'NONE',  ( 2.500000000000000000, -1.178949249685213863, 2.042000000000002924 ) ) ;
#5642 = ORIENTED_EDGE ( 'NONE', *, *, #10214, .F. ) ;
#5643 = FACE_OUTER_BOUND ( 'NONE', #9655, .T. ) ;
#5644 = ORIENTED_EDGE ( 'NONE', *, *, #5684, .T. ) ;
#5645 = VECTOR ( 'NONE', #3069, 1000.000000000000000 ) ;
#5646 = PRESENTATION_LAYER_ASSIGNMENT (  '', '', ( #9013 ) ) ;
#5647 = CARTESIAN_POINT ( 'NONE',  ( -2.472591809326051937, 31.10170313157791000, 16.13843341526694530 ) ) ;
#5648 = CARTESIAN_POINT ( 'NONE',  ( -4.197477534772231955, 0.8522413273724368521, -3.505042416683225692 ) ) ;
#5649 = CARTESIAN_POINT ( 'NONE',  ( 16.89796509758633647, 18.05178237071871195, 12.14735994959122856 ) ) ;
#5650 = DIRECTION ( 'NONE',  ( 0.000000000000000000, 0.000000000000000000, 1.000000000000000000 ) ) ;
#5651 = CARTESIAN_POINT ( 'NONE',  ( -1.243802165048909503, 3.900692638707381921, -3.223146290109805800 ) ) ;
#5652 = CARTESIAN_POINT ( 'NONE',  ( -27.60187600103308014, 51.52708333237728766, -4.064049460664955760 ) ) ;
#5653 = CARTESIAN_POINT ( 'NONE',  ( 4.211140560182196957, -2.431303136016555122, -3.745885042887436622 ) ) ;
#5654 = STYLED_ITEM ( 'NONE', ( #9780 ), #9310 ) ;
#5655 = CARTESIAN_POINT ( 'NONE',  ( 0.1756481739660539498, -4.720212674038995360, -3.469390959564070620 ) ) ;
#5656 = ORIENTED_EDGE ( 'NONE', *, *, #5390, .F. ) ;
#5657 = AXIS2_PLACEMENT_3D ( 'NONE', #9135, #10032, #6417 ) ;
#5658 = DIRECTION ( 'NONE',  ( -1.000000000000000000, 0.000000000000000000, 0.000000000000000000 ) ) ;
#5659 = CARTESIAN_POINT ( 'NONE',  ( -25.98076211353311038, 57.99999999999985789, -9.000000000000701661 ) ) ;
#5660 = ADVANCED_FACE ( 'NONE', ( #9805, #8813, #10482 ), #7930, .T. ) ;
#5661 = CARTESIAN_POINT ( 'NONE',  ( -24.35964822603314417, 49.89374999904394770, -5.000000000000103029 ) ) ;
#5662 = CARTESIAN_POINT ( 'NONE',  ( -27.60187600103308370, 54.96874999904395054, -5.000000000000103029 ) ) ;
#5663 = CARTESIAN_POINT ( 'NONE',  ( 20.46928886811658188, 22.21026755401432240, 11.00732503135576401 ) ) ;
#5664 = CARTESIAN_POINT ( 'NONE',  ( -24.35964822603314772, 55.26041666571062194, -4.064049460664953983 ) ) ;
#5665 = ORIENTED_EDGE ( 'NONE', *, *, #4930, .F. ) ;
#5666 = EDGE_CURVE ( 'NONE', #7952, #3459, #304, .T. ) ;
#5667 = CARTESIAN_POINT ( 'NONE',  ( 34.69563600136375214, 4.609751841799208272, 2.519143709543159471 ) ) ;
#5668 = ORIENTED_EDGE ( 'NONE', *, *, #6000, .T. ) ;
#5669 = CARTESIAN_POINT ( 'NONE',  ( -30.98076211353325249, 14.99999999999984190, -2.500000000000000000 ) ) ;
#5670 = ORIENTED_EDGE ( 'NONE', *, *, #2748, .T. ) ;
#5671 = EDGE_CURVE ( 'NONE', #1617, #6804, #4036, .T. ) ;
#5672 = CARTESIAN_POINT ( 'NONE',  ( -2.385244779468109755E-15, 32.50000000000000711, 16.15625000000000355 ) ) ;
#5673 = EDGE_LOOP ( 'NONE', ( #9154, #2546, #3557, #10620 ) ) ;
#5674 = CARTESIAN_POINT ( 'NONE',  ( 16.98270770525814299, 16.57081904430127395, 11.07189675232624104 ) ) ;
#5675 = CARTESIAN_POINT ( 'NONE',  ( 2.712762565639649015, -3.052587955997662306, -3.430618716626630871 ) ) ;
#5676 = CARTESIAN_POINT ( 'NONE',  ( 17.02848097699435215, 16.52496068989110967, 12.06979569234921890 ) ) ;
#5677 = EDGE_CURVE ( 'NONE', #10983, #1951, #1307, .T. ) ;
#5678 = CARTESIAN_POINT ( 'NONE',  ( -23.98076211353314235, 53.67083333142136325, -6.154700538379337615 ) ) ;
#5679 = DIRECTION ( 'NONE',  ( 1.000000000000000000, -0.000000000000000000, -0.000000000000000000 ) ) ;
#5680 = DIRECTION ( 'NONE',  ( 0.000000000000000000, 0.000000000000000000, -1.000000000000000000 ) ) ;
#5681 = ORIENTED_EDGE ( 'NONE', *, *, #8372, .T. ) ;
#5682 = CARTESIAN_POINT ( 'NONE',  ( -2.500000000000007550, 30.06616922564517580, 17.46655841526694175 ) ) ;
#5683 = ORIENTED_EDGE ( 'NONE', *, *, #460, .T. ) ;
#5684 = EDGE_CURVE ( 'NONE', #7151, #516, #8115, .T. ) ;
#5685 = EDGE_CURVE ( 'NONE', #7847, #7506, #1735, .T. ) ;
#5686 = CARTESIAN_POINT ( 'NONE',  ( 20.11906803080876571, 17.66537948065741759, 13.00425721518307576 ) ) ;
#5687 = CARTESIAN_POINT ( 'NONE',  ( 16.58601566935801586, 18.36373179894819074, 12.17661548709639696 ) ) ;
#5688 = DIRECTION ( 'NONE',  ( -6.098637220230959976E-17, 1.000000000000000000, -2.312964634635742464E-16 ) ) ;
#5689 = CARTESIAN_POINT ( 'NONE',  ( 3.678949249685231848, 0.000000000000000000, 0.000000000000000000 ) ) ;
#5690 = CARTESIAN_POINT ( 'NONE',  ( 1.383578242660657098, 33.52740819067396671, 15.08031658473306891 ) ) ;
#5691 = CARTESIAN_POINT ( 'NONE',  ( 16.23246227876473213, 18.01017840835489991, 12.17661548709639696 ) ) ;
#5692 = ORIENTED_EDGE ( 'NONE', *, *, #10625, .T. ) ;
#5693 = DIRECTION ( 'NONE',  ( 0.000000000000000000, 0.000000000000000000, -1.000000000000000000 ) ) ;
#5694 = EDGE_LOOP ( 'NONE', ( #4363, #4052, #887, #863 ) ) ;
#5695 = CARTESIAN_POINT ( 'NONE',  ( 0.06616922564517249694, 32.50000000000000711, 15.90405841526694175 ) ) ;
#5696 = CARTESIAN_POINT ( 'NONE',  ( 20.05579831881754060, 20.86490736922957367, 2.500000000000000444 ) ) ;
#5697 = DIRECTION ( 'NONE',  ( -1.000000000000000000, 0.000000000000000000, 0.000000000000000000 ) ) ;
#5698 = CARTESIAN_POINT ( 'NONE',  ( 0.000000000000000000, 0.000000000000000000, -4.000000000000000000 ) ) ;
#5699 = EDGE_CURVE ( 'NONE', #5575, #5004, #6504, .T. ) ;
#5700 = CARTESIAN_POINT ( 'NONE',  ( 4.000000000000000000, -1.084202172485504434E-14, -3.142992957459231906 ) ) ;
#5701 = CARTESIAN_POINT ( 'NONE',  ( -24.35964822603314417, 50.41874999904395338, -5.000000000000103029 ) ) ;
#5702 = CARTESIAN_POINT ( 'NONE',  ( 3.199999999999999734, 0.000000000000000000, 3.499999999999999556 ) ) ;
#5703 = CARTESIAN_POINT ( 'NONE',  ( -26.98076211353408382, 57.99999999999985789, -6.732050807568389139 ) ) ;
#5704 = ORIENTED_EDGE ( 'NONE', *, *, #3633, .T. ) ;
#5705 = CARTESIAN_POINT ( 'NONE',  ( 3.500000000000005773, 31.44974746830583001, 14.67187500000000178 ) ) ;
#5706 = FACE_OUTER_BOUND ( 'NONE', #5673, .T. ) ;
#5707 = CARTESIAN_POINT ( 'NONE',  ( -25.98076211353310683, 50.06874999904394485, -6.871901078670399343 ) ) ;
#5708 = CARTESIAN_POINT ( 'NONE',  ( -24.35964822603314417, 53.91874999904395338, -5.000000000000103029 ) ) ;
#5709 = EDGE_CURVE ( 'NONE', #1228, #2958, #9698, .T. ) ;
#5710 = CARTESIAN_POINT ( 'NONE',  ( 22.93505243896877133, 21.90805399618153970, 11.00732503135576401 ) ) ;
#5711 = CARTESIAN_POINT ( 'NONE',  ( -23.98076211353314235, 50.25833333333319075, -6.154700538379337615 ) ) ;
#5712 = ORIENTED_EDGE ( 'NONE', *, *, #10610, .F. ) ;
#5713 =( REPRESENTATION_RELATIONSHIP ('NONE','NONE', #7540, #1223 ) REPRESENTATION_RELATIONSHIP_WITH_TRANSFORMATION ( #2159 )SHAPE_REPRESENTATION_RELATIONSHIP( ) );
#5714 = CARTESIAN_POINT ( 'NONE',  ( -25.98076211353311393, 55.31874999904394485, -3.128098921329806714 ) ) ;
#5715 = ORIENTED_EDGE ( 'NONE', *, *, #1447, .F. ) ;
#5716 = EDGE_LOOP ( 'NONE', ( #9886, #5117, #9939, #5455 ) ) ;
#5717 = CARTESIAN_POINT ( 'NONE',  ( 4.154306624731035846, -2.398490048085128556, -3.721999068284417955 ) ) ;
#5718 = ORIENTED_EDGE ( 'NONE', *, *, #2819, .T. ) ;
#5719 = PLANE ( 'NONE',  #10017 ) ;
#5720 = SURFACE_STYLE_USAGE ( .BOTH. , #42 ) ;
#5721 = VERTEX_POINT ( 'NONE', #7296 ) ;
#5722 = CARTESIAN_POINT ( 'NONE',  ( 20.05551109708751412, 20.00475302350064766, 11.00732503135517426 ) ) ;
#5723 = SURFACE_SIDE_STYLE ('',( #2330 ) ) ;
#5724 = VECTOR ( 'NONE', #1651, 1000.000000000000000 ) ;
#5725 = DIRECTION ( 'NONE',  ( 1.000000000000000000, 0.000000000000000000, 0.000000000000000000 ) ) ;
#5726 = EDGE_CURVE ( 'NONE', #4515, #8667, #1552, .T. ) ;
#5727 = CARTESIAN_POINT ( 'NONE',  ( 19.90085419568980640, 16.36478119802090703, 11.95042571680015442 ) ) ;
#5728 = CARTESIAN_POINT ( 'NONE',  ( -24.98076211353313170, 52.09583333142136752, -3.267949192431250705 ) ) ;
#5729 = CARTESIAN_POINT ( 'NONE',  ( 3.319999999999999840, 0.000000000000000000, 3.249999999999998224 ) ) ;
#5730 = ORIENTED_EDGE ( 'NONE', *, *, #5685, .T. ) ;
#5731 = CARTESIAN_POINT ( 'NONE',  ( -2.474873734152916338, 27.52512626584707789, 14.12500000000000355 ) ) ;
#5732 = ORIENTED_EDGE ( 'NONE', *, *, #6288, .T. ) ;
#5733 = CARTESIAN_POINT ( 'NONE',  ( 23.94195266346560658, 19.36439822498074648, 12.94889058896590583 ) ) ;
#5734 = EDGE_CURVE ( 'NONE', #7593, #2609, #8235, .T. ) ;
#5735 = EDGE_CURVE ( 'NONE', #4007, #670, #833, .T. ) ;
#5736 = CYLINDRICAL_SURFACE ( 'NONE', #2399, 3.500000000000000000 ) ;
#5737 = FACE_OUTER_BOUND ( 'NONE', #7717, .T. ) ;
#5738 = DIRECTION ( 'NONE',  ( 0.000000000000000000, 0.4999999999999989453, -0.8660254037844391517 ) ) ;
#5739 = CARTESIAN_POINT ( 'NONE',  ( 3.472591809326047052, 31.51591669395100936, 14.92406658473306713 ) ) ;
#5740 = DIRECTION ( 'NONE',  ( -1.000000000000000000, 1.224646799147352714E-16, 0.000000000000000000 ) ) ;
#5741 = ORIENTED_EDGE ( 'NONE', *, *, #1068, .T. ) ;
#5742 = PLANE ( 'NONE',  #2262 ) ;
#5743 = ORIENTED_EDGE ( 'NONE', *, *, #6898, .F. ) ;
#5744 = CARTESIAN_POINT ( 'NONE',  ( -1.101703131577911776, 27.52740819067395250, 16.45093341526693820 ) ) ;
#5745 = CARTESIAN_POINT ( 'NONE',  ( 2.100000000000000089, 0.000000000000000000, -4.694516984716113228 ) ) ;
#5746 = CYLINDRICAL_SURFACE ( 'NONE', #9659, 34.99999999999999289 ) ;
#5747 = CARTESIAN_POINT ( 'NONE',  ( 5.791420021395468964, 0.000000000000000000, 3.168237633705329831E-17 ) ) ;
#5748 = DIRECTION ( 'NONE',  ( 0.000000000000000000, 1.000000000000000000, 0.000000000000000000 ) ) ;
#5749 = CARTESIAN_POINT ( 'NONE',  ( -27.60187600103308014, 55.86681177618367400, -4.629976867109323990 ) ) ;
#5750 = CIRCLE ( 'NONE', #10886, 2.500000000000000888 ) ;
#5751 = CARTESIAN_POINT ( 'NONE',  ( 0.3198814748697593746, 4.434118497892183264, -0.3507732604232499107 ) ) ;
#5752 = DIRECTION ( 'NONE',  ( -0.000000000000000000, -0.000000000000000000, -1.000000000000000000 ) ) ;
#5753 = ORIENTED_EDGE ( 'NONE', *, *, #10128, .F. ) ;
#5754 = CARTESIAN_POINT ( 'NONE',  ( -1.734723475976807094E-15, 33.50000000000000000, 14.90625000000000355 ) ) ;
#5755 = CIRCLE ( 'NONE', #599, 4.500000000000000000 ) ;
#5756 = DIRECTION ( 'NONE',  ( 2.775557561562891351E-17, 1.000000000000000000, -8.326672684688671588E-17 ) ) ;
#5757 = SHAPE_REPRESENTATION ( 'socket head cap screw_iso_ISO 4762 M5 x 20 - 20N', ( #308 ), #2282 ) ;
#5758 = AXIS2_PLACEMENT_3D ( 'NONE', #6435, #3890, #1395 ) ;
#5759 = CARTESIAN_POINT ( 'NONE',  ( -26.79131905728310059, 51.06041666571061199, -3.596074190997381237 ) ) ;
#5760 = CARTESIAN_POINT ( 'NONE',  ( -27.60187600103308370, 52.86874999904394912, -5.000000000000103029 ) ) ;
#5761 = CARTESIAN_POINT ( 'NONE',  ( 16.35082997044643704, 18.59891749786092063, 12.19867189564230969 ) ) ;
#5762 = CARTESIAN_POINT ( 'NONE',  ( -27.98076211353308551, 50.49166666666652503, -6.154700538379338504 ) ) ;
#5763 = AXIS2_PLACEMENT_3D ( 'NONE', #371, #1098, #5503 ) ;
#5764 = VERTEX_POINT ( 'NONE', #1633 ) ;
#5765 = CARTESIAN_POINT ( 'NONE',  ( 34.89248166448386002, 2.744837293030728098, 3.511881795860531952 ) ) ;
#5766 = ORIENTED_EDGE ( 'NONE', *, *, #2772, .F. ) ;
#5767 = ORIENTED_EDGE ( 'NONE', *, *, #6000, .F. ) ;
#5768 = CARTESIAN_POINT ( 'NONE',  ( -2.804994570502171047, -3.229033611042465335, -3.526374918436838701 ) ) ;
#5769 = ORIENTED_EDGE ( 'NONE', *, *, #2417, .T. ) ;
#5770 = CARTESIAN_POINT ( 'NONE',  ( -1.767766952966370209, 28.23223304703362402, 15.37500000000000355 ) ) ;
#5771 = AXIS2_PLACEMENT_3D ( 'NONE', #9077, #7413, #10915 ) ;
#5772 = ORIENTED_EDGE ( 'NONE', *, *, #2167, .T. ) ;
#5773 = CARTESIAN_POINT ( 'NONE',  ( 18.58376669197321007, 17.02366754649298031, 11.02344032946268548 ) ) ;
#5774 = AXIS2_PLACEMENT_3D ( 'NONE', #1266, #9816, #7993 ) ;
#5775 = CARTESIAN_POINT ( 'NONE',  ( -4.000000000000000000, 0.000000000000000000, 0.000000000000000000 ) ) ;
#5776 = DIRECTION ( 'NONE',  ( 0.9876851083892502770, 0.1564548710207356030, 0.000000000000000000 ) ) ;
#5777 = CARTESIAN_POINT ( 'NONE',  ( 22.50783536177859645, 18.11075086187001659, 12.94889058896590583 ) ) ;
#5778 = CARTESIAN_POINT ( 'NONE',  ( -24.98076211353312814, 53.02916666475469754, -6.732050807568954909 ) ) ;
#5779 = AXIS2_PLACEMENT_3D ( 'NONE', #3244, #10972, #906 ) ;
#5780 = CARTESIAN_POINT ( 'NONE',  ( 34.74482695545610511, 4.223122737142881888, -2.595677240809973085 ) ) ;
#5781 = DIRECTION ( 'NONE',  ( -1.000000000000000000, -6.098637220230964906E-17, -0.000000000000000000 ) ) ;
#5782 = ORIENTED_EDGE ( 'NONE', *, *, #9399, .T. ) ;
#5783 = CARTESIAN_POINT ( 'NONE',  ( -2.472591809326051937, 31.10170313157791000, 17.38843341526693820 ) ) ;
#5784 = ORIENTED_EDGE ( 'NONE', *, *, #10229, .F. ) ;
#5785 = EDGE_CURVE ( 'NONE', #9280, #101, #9818, .T. ) ;
#5786 = CARTESIAN_POINT ( 'NONE',  ( 18.11095311068464397, 15.98247068297658835, 13.00034071860445550 ) ) ;
#5787 = DIRECTION ( 'NONE',  ( -1.000000000000000000, -0.000000000000000000, -0.000000000000000000 ) ) ;
#5788 = CARTESIAN_POINT ( 'NONE',  ( 2.500000000000000000, 3.004629197474318851E-15, 2.042000000000000259 ) ) ;
#5789 = CARTESIAN_POINT ( 'NONE',  ( 0.000000000000000000, 0.000000000000000000, -4.000000000000000000 ) ) ;
#5790 = CARTESIAN_POINT ( 'NONE',  ( -2.521662442312484931, 32.42808502599334730, 14.06469158473306358 ) ) ;
#5791 = CARTESIAN_POINT ( 'NONE',  ( 0.000000000000000000, 0.000000000000000000, -4.694516984716113228 ) ) ;
#5792 = DIRECTION ( 'NONE',  ( 1.000000000000000000, 6.098637220230963674E-17, -0.000000000000000000 ) ) ;
#5793 = DIRECTION ( 'NONE',  ( -0.000000000000000000, -0.000000000000000000, -1.000000000000000000 ) ) ;
#5794 = ADVANCED_FACE ( 'NONE', ( #10798 ), #5742, .T. ) ;
#5795 = ORIENTED_EDGE ( 'NONE', *, *, #3715, .T. ) ;
#5796 = VERTEX_POINT ( 'NONE', #7516 ) ;
#5797 = CARTESIAN_POINT ( 'NONE',  ( 0.02993401039714972331, 3.373851915354646458, 1.156317065392217680 ) ) ;
#5798 = DIRECTION ( 'NONE',  ( 0.000000000000000000, 0.000000000000000000, -1.000000000000000000 ) ) ;
#5799 = PRODUCT_DEFINITION_SHAPE ( 'NONE', 'NONE',  #10140 ) ;
#5800 = AXIS2_PLACEMENT_3D ( 'NONE', #9180, #5693, #2249 ) ;
#5801 = AXIS2_PLACEMENT_3D ( 'NONE', #207, #9596, #2615 ) ;
#5802 = CARTESIAN_POINT ( 'NONE',  ( 18.27511531525127353, 17.01097670698189290, 12.03680973694848966 ) ) ;
#5803 = DIRECTION ( 'NONE',  ( 0.000000000000000000, 0.000000000000000000, -1.000000000000000000 ) ) ;
#5804 = FACE_OUTER_BOUND ( 'NONE', #2490, .T. ) ;
#5805 = CARTESIAN_POINT ( 'NONE',  ( -27.60187600103308014, 50.01041666571062194, -5.935950539335252074 ) ) ;
#5806 = CARTESIAN_POINT ( 'NONE',  ( 29.50000000000000711, -7.999999999999983125, 17.49999999999999645 ) ) ;
#5807 = CARTESIAN_POINT ( 'NONE',  ( 4.203935335434060505, 1.640780671294165272, -3.598452447879202598 ) ) ;
#5808 = EDGE_CURVE ( 'NONE', #1521, #702, #582, .T. ) ;
#5809 = ORIENTED_EDGE ( 'NONE', *, *, #3168, .T. ) ;
#5810 = VECTOR ( 'NONE', #10560, 1000.000000000000000 ) ;
#5811 = CIRCLE ( 'NONE', #5985, 0.4999999999999985567 ) ;
#5812 = CARTESIAN_POINT ( 'NONE',  ( 3.500000000000005329, 30.00000000000000000, 14.59375000000000178 ) ) ;
#5813 = DIRECTION ( 'NONE',  ( -1.000000000000000000, -6.098637220230963674E-17, 0.000000000000000000 ) ) ;
#5814 = CARTESIAN_POINT ( 'NONE',  ( -27.98076211353308551, 54.04999999999986215, -5.000000000000103029 ) ) ;
#5815 = ADVANCED_FACE ( 'NONE', ( #7405 ), #2407, .T. ) ;
#5816 = CARTESIAN_POINT ( 'NONE',  ( -27.60187600103308725, 51.70208333237728482, -4.064049460664955760 ) ) ;
#5817 = CARTESIAN_POINT ( 'NONE',  ( -27.60187600103308725, 52.11041666571061626, -5.935950539335252074 ) ) ;
#5818 = VECTOR ( 'NONE', #9885, 1000.000000000000000 ) ;
#5819 = MECHANICAL_DESIGN_GEOMETRIC_PRESENTATION_REPRESENTATION (  '', ( #3691 ), #4419 ) ;
#5820 = AXIS2_PLACEMENT_3D ( 'NONE', #1372, #10861, #3251 ) ;
#5821 = CARTESIAN_POINT ( 'NONE',  ( 20.08745147943499987, 17.71083118005251933, 12.00579112326941988 ) ) ;
#5822 = CARTESIAN_POINT ( 'NONE',  ( -26.98076211353309972, 51.83333333333319359, -6.732050807568954909 ) ) ;
#5823 = ORIENTED_EDGE ( 'NONE', *, *, #6672, .T. ) ;
#5824 = FILL_AREA_STYLE_COLOUR ( '', #10092 ) ;
#5825 = ORIENTED_EDGE ( 'NONE', *, *, #4585, .F. ) ;
#5827 = ORIENTED_EDGE ( 'NONE', *, *, #7998, .T. ) ;
#5826 = ADVANCED_FACE ( 'NONE', ( #10738 ), #7577, .F. ) ;
#5828 = CARTESIAN_POINT ( 'NONE',  ( 15.92569759632967497, 17.60983630960342339, 13.17442390236345418 ) ) ;
#5829 = ORIENTED_EDGE ( 'NONE', *, *, #10421, .T. ) ;
#5830 = DIRECTION ( 'NONE',  ( -0.5000000000000016653, 0.8660254037844378194, 0.000000000000000000 ) ) ;
#5831 = ORIENTED_EDGE ( 'NONE', *, *, #2952, .F. ) ;
#5832 = CIRCLE ( 'NONE', #8681, 4.500000000000000888 ) ;
#5833 = CARTESIAN_POINT ( 'NONE',  ( 18.23429108146684641, 17.05446421968790460, 11.03858925989339390 ) ) ;
#5834 = SURFACE_STYLE_USAGE ( .BOTH. , #5723 ) ;
#5835 = LINE ( 'NONE', #6772, #3332 ) ;
#5836 = CARTESIAN_POINT ( 'NONE',  ( 16.42482038756834228, 17.11071351836534049, 12.12541829646253078 ) ) ;
#5837 = FILL_AREA_STYLE ('',( #3277 ) ) ;
#5838 = CARTESIAN_POINT ( 'NONE',  ( -27.98076211353308551, 56.06249999808802897, -5.000000000000103029 ) ) ;
#5839 = LINE ( 'NONE', #112, #788 ) ;
#5840 = ORIENTED_EDGE ( 'NONE', *, *, #5067, .F. ) ;
#5841 = CARTESIAN_POINT ( 'NONE',  ( -25.98076211353311393, 49.49999999999986500, -5.000000000000103029 ) ) ;
#5842 = ORIENTED_EDGE ( 'NONE', *, *, #3905, .F. ) ;
#5843 = CARTESIAN_POINT ( 'NONE',  ( -1.449747468305836229, 33.50000000000000000, 13.73437500000000533 ) ) ;
#5844 = ORIENTED_EDGE ( 'NONE', *, *, #5933, .F. ) ;
#5845 = CARTESIAN_POINT ( 'NONE',  ( 16.77403034288735029, 16.76147925670542094, 13.09486341078152805 ) ) ;
#5846 = CARTESIAN_POINT ( 'NONE',  ( 21.82671760412675610, 17.70440453107251244, 11.95042449705224819 ) ) ;
#5847 = DIRECTION ( 'NONE',  ( 0.000000000000000000, 0.000000000000000000, 1.000000000000000000 ) ) ;
#5848 = DIRECTION ( 'NONE',  ( -0.000000000000000000, -0.000000000000000000, 1.000000000000000000 ) ) ;
#5849 = ADVANCED_FACE ( 'NONE', ( #5643 ), #3515, .T. ) ;
#5850 = CARTESIAN_POINT ( 'NONE',  ( -1.814555661125939912, 31.72097824480680117, 15.31469158473306713 ) ) ;
#5851 = CARTESIAN_POINT ( 'NONE',  ( -23.98076211353314235, 51.51249999808803182, -5.000000000000103029 ) ) ;
#5852 = CARTESIAN_POINT ( 'NONE',  ( 4.000000000000000000, -2.309401076758516691, -0.4999999999999995559 ) ) ;
#5853 = DIRECTION ( 'NONE',  ( -1.000000000000000000, -6.098637220230964906E-17, 0.000000000000000000 ) ) ;
#5854 = VERTEX_POINT ( 'NONE', #6511 ) ;
#5855 = ORIENTED_EDGE ( 'NONE', *, *, #754, .T. ) ;
#5856 = CARTESIAN_POINT ( 'NONE',  ( 0.3208286057739604957, -4.433571671609698228, -0.3503314178412692548 ) ) ;
#5857 = CARTESIAN_POINT ( 'NONE',  ( 3.199999999999999734, 3.031088913245550742, 1.749999999999972466 ) ) ;
#5858 = CARTESIAN_POINT ( 'NONE',  ( 2.474873734152918558, 32.47487373415292211, 13.50000000000000355 ) ) ;
#5859 =( REPRESENTATION_RELATIONSHIP ('NONE','NONE', #7540, #5283 ) REPRESENTATION_RELATIONSHIP_WITH_TRANSFORMATION ( #5442 )SHAPE_REPRESENTATION_RELATIONSHIP( ) );
#5860 = CARTESIAN_POINT ( 'NONE',  ( 4.553649124439118623E-15, 27.49999999999999289, 14.28125000000000355 ) ) ;
#5861 = EDGE_CURVE ( 'NONE', #8097, #10425, #7479, .T. ) ;
#5862 = DIRECTION ( 'NONE',  ( 2.775557561562891351E-17, 1.000000000000000000, -8.326672684688671588E-17 ) ) ;
#5863 = CARTESIAN_POINT ( 'NONE',  ( -27.60187600103308014, 54.50208333237726777, -4.064049460664955760 ) ) ;
#5864 = ADVANCED_FACE ( 'NONE', ( #10079 ), #2470, .F. ) ;
#5865 = CARTESIAN_POINT ( 'NONE',  ( 0.000000000000000000, 0.000000000000000000, 0.000000000000000000 ) ) ;
#5866 = CARTESIAN_POINT ( 'NONE',  ( -25.98076211353310683, 54.13749999808803182, -3.000000000000132339 ) ) ;
#5867 = ORIENTED_EDGE ( 'NONE', *, *, #2480, .F. ) ;
#5868 = CARTESIAN_POINT ( 'NONE',  ( -1.035533905932742638, 32.50000000000000000, 13.73437500000000533 ) ) ;
#5869 = CARTESIAN_POINT ( 'NONE',  ( -25.98076211353311038, 61.49999999999985789, -5.000000000000102141 ) ) ;
#5870 = CARTESIAN_POINT ( 'NONE',  ( -27.60187600103308725, 53.68541666571061199, -5.935950539335252074 ) ) ;
#5871 = EDGE_CURVE ( 'NONE', #4949, #3727, #7398, .T. ) ;
#5872 = CARTESIAN_POINT ( 'NONE',  ( -24.35964822603314417, 51.81874999904395196, -5.000000000000103029 ) ) ;
#5873 = DIRECTION ( 'NONE',  ( -0.7055570967602625698, 0.7055570967602455834, 0.06616922564518108729 ) ) ;
#5874 = CARTESIAN_POINT ( 'NONE',  ( -24.98076211353312814, 51.71666666666652645, -6.732050807568954909 ) ) ;
#5875 = ORIENTED_EDGE ( 'NONE', *, *, #4028, .F. ) ;
#5876 = EDGE_CURVE ( 'NONE', #3723, #4583, #9717, .T. ) ;
#5877 = ADVANCED_FACE ( 'NONE', ( #3961 ), #9916, .T. ) ;
#5878 = ORIENTED_EDGE ( 'NONE', *, *, #1586, .T. ) ;
#5879 = EDGE_LOOP ( 'NONE', ( #3323, #10908, #8084, #7938 ) ) ;
#5880 = LINE ( 'NONE', #7779, #7519 ) ;
#5881 = ORIENTED_EDGE ( 'NONE', *, *, #6656, .F. ) ;
#5882 = CYLINDRICAL_SURFACE ( 'NONE', #967, 1.649999999999995248 ) ;
#5883 = VECTOR ( 'NONE', #7715, 1000.000000000000000 ) ;
#5884 = EDGE_LOOP ( 'NONE', ( #2165, #7160, #4253 ) ) ;
#5885 = CARTESIAN_POINT ( 'NONE',  ( 17.74785087444460885, 17.25574343990722070, 11.06843699004799397 ) ) ;
#5886 = CARTESIAN_POINT ( 'NONE',  ( 5.000000000000004441, 5.204748896376250699E-16, -4.250000000000000000 ) ) ;
#5887 = LINE ( 'NONE', #10114, #1922 ) ;
#5888 = CARTESIAN_POINT ( 'NONE',  ( 20.75790788474667181, 23.61206934513595357, 12.94889058896590583 ) ) ;
#5889 = DIRECTION ( 'NONE',  ( 0.000000000000000000, 0.000000000000000000, 1.000000000000000000 ) ) ;
#5890 = CARTESIAN_POINT ( 'NONE',  ( -27.98076211353308551, 53.96249999808803466, -5.000000000000103029 ) ) ;
#5891 = B_SPLINE_CURVE_WITH_KNOTS ( 'NONE', 3,
 ( #5775, #10113, #7441, #4226, #7615, #7496, #1299, #4060 ),
 .UNSPECIFIED., .F., .F.,
 ( 4, 2, 2, 4 ),
 ( 0.005725059856848641743, 0.006314084072593626612, 0.006903108288338611481, 0.008081156719828581220 ),
 .UNSPECIFIED. ) ;
#5892 = CARTESIAN_POINT ( 'NONE',  ( -25.44486372867087454, 53.55626073911682994, -3.000000000000134559 ) ) ;
#5893 = ORIENTED_EDGE ( 'NONE', *, *, #10640, .F. ) ;
#5894 = CARTESIAN_POINT ( 'NONE',  ( -27.98076211353308551, 50.52083333142136468, -3.845299461620869330 ) ) ;
#5895 = EDGE_LOOP ( 'NONE', ( #7178, #8575, #6347 ) ) ;
#5896 = CARTESIAN_POINT ( 'NONE',  ( -0.06616922564517661864, 33.50000000000000000, 13.90844158473306713 ) ) ;
#5897 = VECTOR ( 'NONE', #7048, 1000.000000000000000 ) ;
#5898 = ORIENTED_EDGE ( 'NONE', *, *, #3844, .T. ) ;
#5899 = ADVANCED_FACE ( 'NONE', ( #6964 ), #3528, .F. ) ;
#5900 = CARTESIAN_POINT ( 'NONE',  ( 20.18549546789347460, 16.49528347911771675, 12.94888893485705061 ) ) ;
#5901 = CARTESIAN_POINT ( 'NONE',  ( -25.18166448601221319, 58.61490192845000990, -6.836013269862629471 ) ) ;
#5902 = DIRECTION ( 'NONE',  ( -1.000000000000000000, -0.000000000000000000, -0.000000000000000000 ) ) ;
#5903 = AXIS2_PLACEMENT_3D ( 'NONE', #10393, #4718, #997 ) ;
#5904 = CARTESIAN_POINT ( 'NONE',  ( -25.17020516978313083, 51.93541666571061910, -6.403925809002825709 ) ) ;
#5905 = CARTESIAN_POINT ( 'NONE',  ( -2.500000000000007550, 31.03553390593274486, 15.14062500000000355 ) ) ;
#5906 = LINE ( 'NONE', #3130, #8260 ) ;
#5907 = CARTESIAN_POINT ( 'NONE',  ( 0.2174200650116529521, -2.185595227305000332, 3.214438021527625811 ) ) ;
#5908 = PLANE ( 'NONE',  #2632 ) ;
#5909 = ORIENTED_EDGE ( 'NONE', *, *, #9998, .T. ) ;
#5910 = ORIENTED_EDGE ( 'NONE', *, *, #3824, .F. ) ;
#5911 = DIRECTION ( 'NONE',  ( 0.000000000000000000, 0.000000000000000000, 1.000000000000000000 ) ) ;
#5912 = CARTESIAN_POINT ( 'NONE',  ( -4.000000000000000000, -0.8382240730041925492, -3.220610619767135141 ) ) ;
#5913 = CARTESIAN_POINT ( 'NONE',  ( 23.31827848602400621, 20.57738196266585362, 12.00579112326941988 ) ) ;
#5914 = CARTESIAN_POINT ( 'NONE',  ( -1.767766952966375094, 31.76776695296636888, 15.06250000000000355 ) ) ;
#5915 = CARTESIAN_POINT ( 'NONE',  ( -25.98076211353311393, 59.49999999999985789, -5.000000000000103029 ) ) ;
#5916 = CARTESIAN_POINT ( 'NONE',  ( -24.35964822603314772, 54.67708333237728624, -5.935950539335252074 ) ) ;
#5917 = CYLINDRICAL_SURFACE ( 'NONE', #6526, 4.500000000000000000 ) ;
#5918 = CARTESIAN_POINT ( 'NONE',  ( -25.36311752100827732, 57.20314267782387674, -3.095295627716787568 ) ) ;
#5919 = FACE_OUTER_BOUND ( 'NONE', #8069, .T. ) ;
#5920 = ORIENTED_EDGE ( 'NONE', *, *, #4324, .T. ) ;
#5921 = DIRECTION ( 'NONE',  ( 6.098637220230963674E-17, -1.000000000000000000, 0.000000000000000000 ) ) ;
#5922 = CARTESIAN_POINT ( 'NONE',  ( -25.17020516978313083, 53.51041666571060773, -6.403925809002825709 ) ) ;
#5923 = VECTOR ( 'NONE', #10703, 1000.000000000000114 ) ;
#5924 = CARTESIAN_POINT ( 'NONE',  ( -4.000000000000000000, -2.309401076758515803, -0.4999999999999995559 ) ) ;
#5925 = CARTESIAN_POINT ( 'NONE',  ( 3.200000000000000178, -2.020725942163647648, 3.499999999999999556 ) ) ;
#5926 = CARTESIAN_POINT ( 'NONE',  ( -26.98076211353309972, 53.93333333333319501, -6.732050807568954909 ) ) ;
#5927 = EDGE_LOOP ( 'NONE', ( #4950, #10052, #6499, #1671 ) ) ;
#5928 = ADVANCED_FACE ( 'NONE', ( #2583, #10966 ), #5908, .T. ) ;
#5929 = ORIENTED_EDGE ( 'NONE', *, *, #1202, .T. ) ;
#5930 = VECTOR ( 'NONE', #6096, 1000.000000000000000 ) ;
#5931 = ORIENTED_EDGE ( 'NONE', *, *, #3771, .T. ) ;
#5932 = PLANE ( 'NONE',  #3970 ) ;
#5934 = ORIENTED_EDGE ( 'NONE', *, *, #10248, .T. ) ;
#5933 = EDGE_CURVE ( 'NONE', #10159, #5073, #5304, .T. ) ;
#5935 = CARTESIAN_POINT ( 'NONE',  ( 0.000000000000000000, 30.00000000000000000, -23.71320343559643007 ) ) ;
#5936 =( NAMED_UNIT ( * ) PLANE_ANGLE_UNIT ( ) SI_UNIT ( $, .RADIAN. ) );
#5937 = ORIENTED_EDGE ( 'NONE', *, *, #9425, .F. ) ;
#5938 = CARTESIAN_POINT ( 'NONE',  ( 21.42382487881899777, 22.58916947935290764, 11.00732503135576401 ) ) ;
#5939 = CARTESIAN_POINT ( 'NONE',  ( 29.49999999999999645, -17.99999999999998579, 7.500000000000053291 ) ) ;
#5940 = ADVANCED_FACE ( 'NONE', ( #9459 ), #7808, .F. ) ;
#5941 = LINE ( 'NONE', #7837, #6292 ) ;
#5942 = CIRCLE ( 'NONE', #7542, 2.649999999999992362 ) ;
#5943 = DIRECTION ( 'NONE',  ( 0.000000000000000000, 0.000000000000000000, 1.000000000000000000 ) ) ;
#5944 = CARTESIAN_POINT ( 'NONE',  ( 22.47621881040483771, 18.15620256126511478, 11.95042449705224819 ) ) ;
#5945 = PLANE ( 'NONE',  #10792 ) ;
#5946 = CARTESIAN_POINT ( 'NONE',  ( -27.60187600103308370, 50.24374999904394912, -5.000000000000103029 ) ) ;
#5947 = CIRCLE ( 'NONE', #4357, 4.999999999999997335 ) ;
#5948 = CYLINDRICAL_SURFACE ( 'NONE', #6305, 24.99999999999999645 ) ;
#5949 = ORIENTED_EDGE ( 'NONE', *, *, #2900, .T. ) ;
#5950 = CARTESIAN_POINT ( 'NONE',  ( -25.98076211353311393, 50.28749999808804461, -7.000000000000073719 ) ) ;
#5951 = ORIENTED_EDGE ( 'NONE', *, *, #2832, .T. ) ;
#5952 = AXIS2_PLACEMENT_3D ( 'NONE', #9738, #5303, #447 ) ;
#5953 = CARTESIAN_POINT ( 'NONE',  ( 2.428085025993350410, 32.52166244231248271, 15.00219158473306535 ) ) ;
#5954 = AXIS2_PLACEMENT_3D ( 'NONE', #6696, #1588, #7472 ) ;
#5955 = ORIENTED_EDGE ( 'NONE', *, *, #685, .T. ) ;
#5956 = CARTESIAN_POINT ( 'NONE',  ( 17.43584335925693196, 16.24128823292743817, 13.04062965360331106 ) ) ;
#5957 = DIRECTION ( 'NONE',  ( 1.000000000000000000, -0.000000000000000000, -0.000000000000000000 ) ) ;
#5958 = CARTESIAN_POINT ( 'NONE',  ( 18.79784185921769790, 16.99560944861731215, 12.01584860934582366 ) ) ;
#5960 = CARTESIAN_POINT ( 'NONE',  ( -24.35964822603314772, 51.76041666571060773, -4.064049460664953983 ) ) ;
#5959 = AXIS2_PLACEMENT_3D ( 'NONE', #3814, #9762, #10909 ) ;
#5961 = CARTESIAN_POINT ( 'NONE',  ( 1.767766952966372429, 31.76776695296637598, 16.00000000000000355 ) ) ;
#5962 = FACE_OUTER_BOUND ( 'NONE', #7379, .T. ) ;
#5963 = CARTESIAN_POINT ( 'NONE',  ( 34.99999999999999289, -3.999999999999993339, -4.999999999999995559 ) ) ;
#5964 = CARTESIAN_POINT ( 'NONE',  ( 2.000000000000000000, 0.8865213383406680414, -1.535500000000000975 ) ) ;
#5965 = ORIENTED_EDGE ( 'NONE', *, *, #10813, .T. ) ;
#5966 = VERTEX_POINT ( 'NONE', #3357 ) ;
#5967 = EDGE_CURVE ( 'NONE', #9110, #183, #1376, .T. ) ;
#5968 = DIRECTION ( 'NONE',  ( 1.000000000000000000, 0.000000000000000000, 0.000000000000000000 ) ) ;
#5969 = CIRCLE ( 'NONE', #2241, 3.499999999999999556 ) ;
#5970 = DIRECTION ( 'NONE',  ( 1.000000000000000000, 0.000000000000000000, 0.000000000000000000 ) ) ;
#5971 = CARTESIAN_POINT ( 'NONE',  ( 23.13231036272843966, 20.08340223762181154, 12.00579112326941988 ) ) ;
#5972 = CARTESIAN_POINT ( 'NONE',  ( -2.500000000000005773, 29.99999999999999645, 15.21875000000000355 ) ) ;
#5973 = LINE ( 'NONE', #7757, #1444 ) ;
#5974 = CARTESIAN_POINT ( 'NONE',  ( -24.35964822603314417, 54.61874999904395622, -5.000000000000103029 ) ) ;
#5975 = FILL_AREA_STYLE_COLOUR ( '', #7410 ) ;
#5976 = CARTESIAN_POINT ( 'NONE',  ( -25.98076211353311393, 49.49999999999986500, -5.000000000000103029 ) ) ;
#5977 = CARTESIAN_POINT ( 'NONE',  ( 4.000000000000000000, 1.680228229147133767, -3.316631783032546021 ) ) ;
#5978 = ORIENTED_EDGE ( 'NONE', *, *, #3883, .F. ) ;
#5979 = CARTESIAN_POINT ( 'NONE',  ( -26.51666049839535333, 50.69373926088290006, -3.000000000000132783 ) ) ;
#5980 = DIRECTION ( 'NONE',  ( 0.000000000000000000, 0.000000000000000000, 1.000000000000000000 ) ) ;
#5981 = CARTESIAN_POINT ( 'NONE',  ( -27.60187600103308370, 55.14374999904394059, -5.000000000000103029 ) ) ;
#5982 = FACE_OUTER_BOUND ( 'NONE', #8646, .T. ) ;
#5983 = CARTESIAN_POINT ( 'NONE',  ( 2.500000000000000000, 1.768423874527824902, 1.020999999999999019 ) ) ;
#5984 = AXIS2_PLACEMENT_3D ( 'NONE', #10300, #1852, #5192 ) ;
#5985 = AXIS2_PLACEMENT_3D ( 'NONE', #6177, #7959, #7120 ) ;
#5986 = CARTESIAN_POINT ( 'NONE',  ( -23.98076211353314235, 53.64166666666653072, -3.845299461620867554 ) ) ;
#5987 = ORIENTED_EDGE ( 'NONE', *, *, #6598, .F. ) ;
#5988 = EDGE_CURVE ( 'NONE', #4348, #6258, #6334, .T. ) ;
#5989 = EDGE_LOOP ( 'NONE', ( #4760, #2797, #2170, #9518, #6880 ) ) ;
#5990 = DIRECTION ( 'NONE',  ( 0.000000000000000000, -0.4999999999999989453, 0.8660254037844391517 ) ) ;
#5991 = DIRECTION ( 'NONE',  ( -0.5000000000000061062, 0.000000000000000000, 0.8660254037844351549 ) ) ;
#5992 = PRODUCT_CONTEXT ( 'NONE', #10820, 'mechanical' ) ;
#5993 = ORIENTED_EDGE ( 'NONE', *, *, #1888, .F. ) ;
#5995 = DIRECTION ( 'NONE',  ( -0.000000000000000000, -0.000000000000000000, 1.000000000000000000 ) ) ;
#5994 = AXIS2_PLACEMENT_3D ( 'NONE', #999, #10176, #55 ) ;
#5996 = CARTESIAN_POINT ( 'NONE',  ( 3.170065989602862455, 3.373851915354605602, -1.156317065392272303 ) ) ;
#5997 = CARTESIAN_POINT ( 'NONE',  ( 29.49999999999999289, 2.000000000000001776, -2.500000000000000000 ) ) ;
#5998 = AXIS2_PLACEMENT_3D ( 'NONE', #6922, #10311, #140 ) ;
#5999 = CARTESIAN_POINT ( 'NONE',  ( -4.000000000000000000, -2.309401076758512694, -3.433295621305382461 ) ) ;
#6000 = EDGE_CURVE ( 'NONE', #7474, #2160, #5249, .T. ) ;
#6001 = CARTESIAN_POINT ( 'NONE',  ( 23.34652552892808330, 18.77429515943753202, 11.95042449705224819 ) ) ;
#6002 = CARTESIAN_POINT ( 'NONE',  ( -1.734723475976807094E-15, 33.50000000000000000, 16.15625000000000355 ) ) ;
#6003 = EDGE_CURVE ( 'NONE', #7695, #10667, #4578, .T. ) ;
#6004 = CARTESIAN_POINT ( 'NONE',  ( -24.35964822603314772, 50.65208333237728056, -5.935950539335252074 ) ) ;
#6005 = CARTESIAN_POINT ( 'NONE',  ( 29.49999999999999645, -3.999999999999993339, -4.999999999999995559 ) ) ;
#6006 = ORIENTED_EDGE ( 'NONE', *, *, #10319, .F. ) ;
#6007 = DIRECTION ( 'NONE',  ( -6.098637220230963674E-17, 1.000000000000000000, 0.000000000000000000 ) ) ;
#6008 = ORIENTED_EDGE ( 'NONE', *, *, #9335, .T. ) ;
#6009 = AXIS2_PLACEMENT_3D ( 'NONE', #3030, #4230, #8184 ) ;
#6010 = CARTESIAN_POINT ( 'NONE',  ( -1.449747468305830678, 26.49999999999999289, 15.45312500000000178 ) ) ;
#6011 = VERTEX_POINT ( 'NONE', #6913 ) ;
#6012 = CARTESIAN_POINT ( 'NONE',  ( 16.42482038756834228, 17.11071351836534049, 12.12541829646253078 ) ) ;
#6013 =( LENGTH_UNIT ( ) NAMED_UNIT ( * ) SI_UNIT ( .MILLI., .METRE. ) );
#6014 = ADVANCED_FACE ( 'NONE', ( #6020, #8690 ), #4362, .F. ) ;
#6015 = CARTESIAN_POINT ( 'NONE',  ( 16.42482038756834228, 17.11071351836534049, 12.12541829646253078 ) ) ;
#6016 = CARTESIAN_POINT ( 'NONE',  ( 19.84380896203909828, 21.37294244821887546, 12.00579112326902731 ) ) ;
#6017 = CARTESIAN_POINT ( 'NONE',  ( -25.98076211353311393, 50.24374999904395622, -3.128098921329806714 ) ) ;
#6018 = CARTESIAN_POINT ( 'NONE',  ( -2.500000000000007550, 31.03553390593274486, 13.89062500000000355 ) ) ;
#6019 = PLANE ( 'NONE',  #1147 ) ;
#6020 = FACE_BOUND ( 'NONE', #10614, .T. ) ;
#6021 = EDGE_CURVE ( 'NONE', #6545, #3095, #6875, .T. ) ;
#6022 = VERTEX_POINT ( 'NONE', #9405 ) ;
#6023 = ADVANCED_FACE ( 'NONE', ( #11 ), #134, .T. ) ;
#6024 = ORIENTED_EDGE ( 'NONE', *, *, #7878, .T. ) ;
#6025 = DIRECTION ( 'NONE',  ( -1.000000000000000000, 0.000000000000000000, 0.000000000000000000 ) ) ;
#6026 = DIRECTION ( 'NONE',  ( 0.000000000000000000, 0.000000000000000000, -1.000000000000000000 ) ) ;
#6027 = CARTESIAN_POINT ( 'NONE',  ( 34.80704760714189661, 3.674543421742908045, -2.801642449272108149 ) ) ;
#6028 = CARTESIAN_POINT ( 'NONE',  ( -1.035533905932742860, 32.50000000000000000, 16.23437500000000355 ) ) ;
#6029 = CARTESIAN_POINT ( 'NONE',  ( 3.472371940585993855, 2.614027278893175321, -3.320322319201766792 ) ) ;
#6030 = CARTESIAN_POINT ( 'NONE',  ( -27.60187600103308370, 54.26874999904394770, -5.000000000000103029 ) ) ;
#6031 = DIRECTION ( 'NONE',  ( -1.000000000000000000, -0.000000000000000000, -0.000000000000000000 ) ) ;
#6032 = CARTESIAN_POINT ( 'NONE',  ( -25.98076211353311749, 56.99999999999886313, -3.000000000000122569 ) ) ;
#6033 = LINE ( 'NONE', #301, #8624 ) ;
#6034 = EDGE_LOOP ( 'NONE', ( #6904, #4408, #6262, #5844 ) ) ;
#6035 = CARTESIAN_POINT ( 'NONE',  ( -25.98076211353310683, 54.13749999808803182, -3.000000000000132339 ) ) ;
#6036 = CARTESIAN_POINT ( 'NONE',  ( -25.98076211353311038, 61.49999999999985789, -5.000000000000102141 ) ) ;
#6037 = CARTESIAN_POINT ( 'NONE',  ( -25.98076211353311393, 53.08749999808803466, -7.000000000000072831 ) ) ;
#6038 = EDGE_CURVE ( 'NONE', #10425, #7419, #4936, .T. ) ;
#6039 = CARTESIAN_POINT ( 'NONE',  ( -24.35964822603314772, 53.45208333237727771, -5.935950539335252074 ) ) ;
#6040 = LINE ( 'NONE', #4496, #9439 ) ;
#6041 = FACE_OUTER_BOUND ( 'NONE', #261, .T. ) ;
#6042 = ORIENTED_EDGE ( 'NONE', *, *, #8615, .T. ) ;
#6043 = ORIENTED_EDGE ( 'NONE', *, *, #2218, .F. ) ;
#6044 = CARTESIAN_POINT ( 'NONE',  ( 0.3126073911696294338, 2.020725942163657862, -3.499999999999999556 ) ) ;
#6045 = FACE_OUTER_BOUND ( 'NONE', #6034, .T. ) ;
#6046 = EDGE_LOOP ( 'NONE', ( #10377, #10219, #2191, #9817, #3937, #5670 ) ) ;
#6047 = CARTESIAN_POINT ( 'NONE',  ( 5.200000000000002842, 0.000000000000000000, -2.700000000000001066 ) ) ;
#6048 = AXIS2_PLACEMENT_3D ( 'NONE', #794, #3191, #10747 ) ;
#6049 = EDGE_CURVE ( 'NONE', #3226, #5586, #10187, .T. ) ;
#6050 = LINE ( 'NONE', #993, #8961 ) ;
#6051 =( BOUNDED_CURVE ( )  B_SPLINE_CURVE ( 2, ( #3606, #10546, #8764, #1041, #9711, #7941, #1947, #10327, #367 ),
 .UNSPECIFIED., .F., .F. ) 
 B_SPLINE_CURVE_WITH_KNOTS ( ( 3, 2, 2, 2, 3 ),
 ( 0.8055555555555555802, 0.8148148148148147696, 0.8333333333333333703, 0.8518518518518518601, 0.8611111111111111605 ),
 .UNSPECIFIED. ) 
 CURVE ( )  GEOMETRIC_REPRESENTATION_ITEM ( )  RATIONAL_B_SPLINE_CURVE ( ( 0.9330127018922194093, 0.9330127018922197424, 1.000000000000000000, 0.8660254037844387076, 1.000000000000000000, 0.8660254037844387076, 1.000000000000000000, 0.9330127018922189652, 0.9330127018922194093 ) ) 
 REPRESENTATION_ITEM ( '' )  );
#6052 = CARTESIAN_POINT ( 'NONE',  ( 19.79393261808261428, 23.04652112618272852, 11.95042449705224819 ) ) ;
#6053 = LINE ( 'NONE', #9441, #7484 ) ;
#6054 = CARTESIAN_POINT ( 'NONE',  ( -23.98076211353314235, 55.01249999808803182, -5.000000000000103029 ) ) ;
#6055 = CONICAL_SURFACE ( 'NONE', #8180, 2.767949192431121919, 0.5235987755982959291 ) ;
#6056 = DIRECTION ( 'NONE',  ( -0.000000000000000000, -0.000000000000000000, -1.000000000000000000 ) ) ;
#6057 = VERTEX_POINT ( 'NONE', #3472 ) ;
#6058 = CARTESIAN_POINT ( 'NONE',  ( 24.30992024302469900, 5.833333333333334814, -2.500000000000000000 ) ) ;
#6059 = ORIENTED_EDGE ( 'NONE', *, *, #693, .T. ) ;
#6060 = CARTESIAN_POINT ( 'NONE',  ( -3.472591809326043499, 28.48408330604899064, 14.29906658473306358 ) ) ;
#6061 = ORIENTED_EDGE ( 'NONE', *, *, #7153, .T. ) ;
#6062 = CARTESIAN_POINT ( 'NONE',  ( 20.77365933115271446, 23.55783661745384094, 11.95042449705224819 ) ) ;
#6063 =( NAMED_UNIT ( * ) PLANE_ANGLE_UNIT ( ) SI_UNIT ( $, .RADIAN. ) );
#6064 = CARTESIAN_POINT ( 'NONE',  ( 29.17190429162964094, 7.000000000000002665, 2.500000000000000000 ) ) ;
#6065 = CARTESIAN_POINT ( 'NONE',  ( 15.92724728075741680, 19.02250018754875072, 13.24059312800850030 ) ) ;
#6066 = CARTESIAN_POINT ( 'NONE',  ( -24.35964822603314417, 50.41874999904395338, -5.000000000000103029 ) ) ;
#6067 = CARTESIAN_POINT ( 'NONE',  ( -2.385244779468109755E-15, 32.50000000000000711, 14.90625000000000355 ) ) ;
#6068 = AXIS2_PLACEMENT_3D ( 'NONE', #940, #1899, #1103 ) ;
#6069 = DIRECTION ( 'NONE',  ( 1.000000000000000000, -0.000000000000000000, 1.156482317317871478E-16 ) ) ;
#6070 = CARTESIAN_POINT ( 'NONE',  ( 11.99999999999999645, 0.000000000000000000, 0.000000000000000000 ) ) ;
#6071 = ORIENTED_EDGE ( 'NONE', *, *, #2056, .F. ) ;
#6072 = EDGE_CURVE ( 'NONE', #3184, #2547, #10788, .T. ) ;
#6073 = VERTEX_POINT ( 'NONE', #3793 ) ;
#6074 = ADVANCED_FACE ( 'NONE', ( #7915 ), #4524, .T. ) ;
#6075 = CARTESIAN_POINT ( 'NONE',  ( 19.13264607096459002, 17.09257730534942965, 12.00833071292064425 ) ) ;
#6076 = CARTESIAN_POINT ( 'NONE',  ( -25.98076211353311393, 52.73749999808803324, -3.000000000000132783 ) ) ;
#6077 = CARTESIAN_POINT ( 'NONE',  ( 19.55162244606592381, 17.33808635661342024, 12.00579012602852735 ) ) ;
#6078 = AXIS2_PLACEMENT_3D ( 'NONE', #2789, #4459, #7840 ) ;
#6079 = CARTESIAN_POINT ( 'NONE',  ( -24.98076211353313170, 55.59583333142136752, -3.267949192431250705 ) ) ;
#6080 = FACE_BOUND ( 'NONE', #2320, .T. ) ;
#6081 = CARTESIAN_POINT ( 'NONE',  ( -25.17020516978313083, 52.63541666571061484, -6.403925809002825709 ) ) ;
#6082 = DIRECTION ( 'NONE',  ( 0.000000000000000000, 0.4999999999999989453, -0.8660254037844391517 ) ) ;
#6083 = CARTESIAN_POINT ( 'NONE',  ( -25.00806794893706453, 57.73399265161810945, -3.251554382635098772 ) ) ;
#6084 = CARTESIAN_POINT ( 'NONE',  ( 5.000000000000004441, 0.000000000000000000, 4.250000000000000000 ) ) ;
#6085 = ORIENTED_EDGE ( 'NONE', *, *, #8721, .F. ) ;
#6086 = PRESENTATION_STYLE_ASSIGNMENT (( #10367 ) ) ;
#6087 = CARTESIAN_POINT ( 'NONE',  ( 2.527408190673967159, 30.96936468028756906, 16.91968341526693820 ) ) ;
#6088 = FACE_OUTER_BOUND ( 'NONE', #265, .T. ) ;
#6089 = CARTESIAN_POINT ( 'NONE',  ( -27.60187600103308370, 53.04374999904394627, -5.000000000000103029 ) ) ;
#6090 = CARTESIAN_POINT ( 'NONE',  ( -25.98076211353311393, 49.49999999999986500, -7.000000000000074607 ) ) ;
#6091 = DIRECTION ( 'NONE',  ( 0.000000000000000000, 0.8660254037844316022, -0.5000000000000124345 ) ) ;
#6092 = DIRECTION ( 'NONE',  ( -1.000000000000000000, -0.000000000000000000, -0.000000000000000000 ) ) ;
#6093 = VERTEX_POINT ( 'NONE', #9683 ) ;
#6094 = ORIENTED_EDGE ( 'NONE', *, *, #3519, .T. ) ;
#6095 = CARTESIAN_POINT ( 'NONE',  ( 34.99999999999987210, -7.999999999999983125, 17.49999999999999645 ) ) ;
#6096 = DIRECTION ( 'NONE',  ( 6.098637220230963674E-17, -1.000000000000000000, 0.000000000000000000 ) ) ;
#6097 = SHAPE_DEFINITION_REPRESENTATION ( #7582, #7975 ) ;
#6098 = ORIENTED_EDGE ( 'NONE', *, *, #10009, .F. ) ;
#6099 = EDGE_CURVE ( 'NONE', #6333, #5356, #4634, .T. ) ;
#6100 = CARTESIAN_POINT ( 'NONE',  ( 2.804994570502171047, 3.229033611042449792, -3.526374918436834704 ) ) ;
#6101 = CARTESIAN_POINT ( 'NONE',  ( -24.98076211353312814, 54.51666666666653072, -6.732050807568954909 ) ) ;
#6102 = CARTESIAN_POINT ( 'NONE',  ( 22.08651808663882932, 17.88512374315008557, 11.95042449705224819 ) ) ;
#6103 = CIRCLE ( 'NONE', #8600, 1.610000000000000098 ) ;
#6104 = CYLINDRICAL_SURFACE ( 'NONE', #8919, 2.000000000000000000 ) ;
#6105 = CARTESIAN_POINT ( 'NONE',  ( -25.98076211353311393, 52.16874999904393917, -6.871901078670400231 ) ) ;
#6106 = FACE_OUTER_BOUND ( 'NONE', #4017, .T. ) ;
#6107 = ORIENTED_EDGE ( 'NONE', *, *, #8988, .T. ) ;
#6108 = DIRECTION ( 'NONE',  ( 1.000000000000000000, 0.000000000000000000, 0.000000000000000000 ) ) ;
#6109 = VERTEX_POINT ( 'NONE', #5574 ) ;
#6110 = CARTESIAN_POINT ( 'NONE',  ( -2.521662442312484931, 32.42808502599334730, 15.31469158473306713 ) ) ;
#6111 = CIRCLE ( 'NONE', #7175, 4.999999999999997335 ) ;
#6112 = ORIENTED_EDGE ( 'NONE', *, *, #10758, .F. ) ;
#6113 = CARTESIAN_POINT ( 'NONE',  ( 22.60611905166032898, 18.24656216730335601, 11.95042449705224819 ) ) ;
#6114 =( BOUNDED_CURVE ( )  B_SPLINE_CURVE ( 2, ( #7709, #10924, #3256, #7534, #5814, #2603, #3374, #5213, #85 ),
 .UNSPECIFIED., .F., .F. ) 
 B_SPLINE_CURVE_WITH_KNOTS ( ( 3, 2, 2, 2, 3 ),
 ( 0.6944444444444445308, 0.7037037037037037202, 0.7222222222222222099, 0.7407407407407406996, 0.7500000000000000000 ),
 .UNSPECIFIED. ) 
 CURVE ( )  GEOMETRIC_REPRESENTATION_ITEM ( )  RATIONAL_B_SPLINE_CURVE ( ( 0.9330127018922194093, 0.9330127018922197424, 1.000000000000000000, 0.8660254037844387076, 1.000000000000000000, 0.8660254037844387076, 1.000000000000000000, 0.9330127018922194093, 0.9330127018922194093 ) ) 
 REPRESENTATION_ITEM ( '' )  );
#6115 = AXIS2_PLACEMENT_3D ( 'NONE', #4091, #7708, #6805 ) ;
#6116 = CARTESIAN_POINT ( 'NONE',  ( 22.43871220627207563, 23.52649944903870249, 11.95042449705224819 ) ) ;
#6117 = CARTESIAN_POINT ( 'NONE',  ( 16.74199038346592872, 18.20775708483950694, 12.16198771834549497 ) ) ;
#6118 = CARTESIAN_POINT ( 'NONE',  ( -24.35964822603314772, 51.17708333237728624, -5.935950539335252074 ) ) ;
#6119 = VECTOR ( 'NONE', #9946, 1000.000000000000000 ) ;
#6120 = VECTOR ( 'NONE', #4633, 1000.000000000000000 ) ;
#6121 =( NAMED_UNIT ( * ) PLANE_ANGLE_UNIT ( ) SI_UNIT ( $, .RADIAN. ) );
#6122 = CIRCLE ( 'NONE', #4387, 3.499999999999999556 ) ;
#6123 = CIRCLE ( 'NONE', #2759, 0.2000000000000000944 ) ;
#6124 = CARTESIAN_POINT ( 'NONE',  ( -25.98076211353311393, 52.38749999808802471, -7.000000000000072831 ) ) ;
#6125 = CARTESIAN_POINT ( 'NONE',  ( -26.48707796582369056, 58.87212001354424018, -6.938716998541621273 ) ) ;
#6126 = ORIENTED_EDGE ( 'NONE', *, *, #10009, .T. ) ;
#6127 = ORIENTED_EDGE ( 'NONE', *, *, #4928, .F. ) ;
#6128 = CARTESIAN_POINT ( 'NONE',  ( -25.98076211353311393, 49.49999999999986500, -5.000000000000103029 ) ) ;
#6129 = CIRCLE ( 'NONE', #5771, 3.499999999999997780 ) ;
#6130 = CARTESIAN_POINT ( 'NONE',  ( -25.98076211353311393, 49.49999999999986500, -5.000000000000103029 ) ) ;
#6131 = CARTESIAN_POINT ( 'NONE',  ( -24.98076211353312814, 50.31666666666652787, -6.732050807568954909 ) ) ;
#6132 = DIRECTION ( 'NONE',  ( 0.000000000000000000, 0.000000000000000000, 1.000000000000000000 ) ) ;
#6133 = LINE ( 'NONE', #2594, #4473 ) ;
#6134 = CARTESIAN_POINT ( 'NONE',  ( -24.35964822603314772, 52.57708333237728482, -5.935950539335252074 ) ) ;
#6135 = EDGE_CURVE ( 'NONE', #4811, #4391, #6284, .T. ) ;
#6136 = DIRECTION ( 'NONE',  ( 1.000000000000000000, 0.000000000000000000, 0.000000000000000000 ) ) ;
#6137 = CARTESIAN_POINT ( 'NONE',  ( -3.974344831685191280E-13, 4.796734841935104576, -3.721909803043223608 ) ) ;
#6138 = LINE ( 'NONE', #1132, #2778 ) ;
#6139 = ORIENTED_EDGE ( 'NONE', *, *, #10269, .F. ) ;
#6140 = FILL_AREA_STYLE ('',( #8320 ) ) ;
#6141 = ADVANCED_FACE ( 'NONE', ( #10575 ), #2018, .F. ) ;
#6142 = AXIS2_PLACEMENT_3D ( 'NONE', #4607, #2881, #4657 ) ;
#6143 = CARTESIAN_POINT ( 'NONE',  ( -2.527408190673963162, 29.03063531971243094, 16.29468341526694530 ) ) ;
#6144 = CARTESIAN_POINT ( 'NONE',  ( -2.500000000000007550, 31.03553390593274486, 16.39062500000000355 ) ) ;
#6145 = CARTESIAN_POINT ( 'NONE',  ( 29.49999999999999645, -9.999999999999998224, -10.50000000000000355 ) ) ;
#6146 = DIRECTION ( 'NONE',  ( 1.000000000000000000, 0.000000000000000000, 0.000000000000000000 ) ) ;
#6147 = EDGE_CURVE ( 'NONE', #4773, #5606, #1177, .T. ) ;
#6148 = AXIS2_PLACEMENT_3D ( 'NONE', #3245, #10192, #10138 ) ;
#6149 = DIRECTION ( 'NONE',  ( -1.000000000000000000, -6.098637220230963674E-17, 0.000000000000000000 ) ) ;
#6150 = DIRECTION ( 'NONE',  ( 0.000000000000000000, 1.000000000000000000, 1.224646799147353207E-16 ) ) ;
#6151 = ORIENTED_EDGE ( 'NONE', *, *, #7653, .T. ) ;
#6152 =( GEOMETRIC_REPRESENTATION_CONTEXT ( 3 ) GLOBAL_UNCERTAINTY_ASSIGNED_CONTEXT ( ( #1875 ) ) GLOBAL_UNIT_ASSIGNED_CONTEXT ( ( #4788, #6547, #7274 ) ) REPRESENTATION_CONTEXT ( 'NONE', 'WORKASPACE' ) );
#6153 = ORIENTED_EDGE ( 'NONE', *, *, #7918, .T. ) ;
#6154 = CARTESIAN_POINT ( 'NONE',  ( 4.750000000000000888, 0.000000000000000000, 3.249999999999999112 ) ) ;
#6155 = EDGE_CURVE ( 'NONE', #4873, #5523, #2293, .T. ) ;
#6156 = DIRECTION ( 'NONE',  ( 0.000000000000000000, 0.000000000000000000, 1.000000000000000000 ) ) ;
#6157 = DIRECTION ( 'NONE',  ( 0.000000000000000000, -1.000000000000000000, 0.000000000000000000 ) ) ;
#6158 = ORIENTED_EDGE ( 'NONE', *, *, #7702, .F. ) ;
#6159 = CARTESIAN_POINT ( 'NONE',  ( 2.000000000000000000, 1.773042676681340524, -2.059984127722458425E-15 ) ) ;
#6160 = DIRECTION ( 'NONE',  ( -1.000000000000000000, 0.000000000000000000, 0.000000000000000000 ) ) ;
#6161 = AXIS2_PLACEMENT_3D ( 'NONE', #4810, #8188, #564 ) ;
#6162 = DIRECTION ( 'NONE',  ( 0.000000000000000000, 0.000000000000000000, -1.000000000000000000 ) ) ;
#6163 = CARTESIAN_POINT ( 'NONE',  ( 18.02930464311577907, 16.06944570838860642, 11.00389976449426399 ) ) ;
#6164 = ADVANCED_FACE ( 'NONE', ( #10408 ), #7080, .T. ) ;
#6165 = CARTESIAN_POINT ( 'NONE',  ( 24.49999999999999289, -3.999999999999986233, -4.999999999999992006 ) ) ;
#6166 = CARTESIAN_POINT ( 'NONE',  ( -24.35964822603314417, 54.09374999904395054, -5.000000000000103029 ) ) ;
#6167 = CARTESIAN_POINT ( 'NONE',  ( 2.500000000000000000, -1.178949249685213863, 2.042000000000002924 ) ) ;
#6168 = VERTEX_POINT ( 'NONE', #6184 ) ;
#6169 = CARTESIAN_POINT ( 'NONE',  ( 6.015568632492064083, 34.47916666666664298, 0.000000000000000000 ) ) ;
#6170 =( BOUNDED_SURFACE ( )  B_SPLINE_SURFACE ( 3, 2, ( 
 ( #9705, #10597, #2994 ),
 ( #8195, #5594, #8980 ),
 ( #5651, #1370, #1424 ),
 ( #4817, #6253, #2040 ),
 ( #5434, #10541, #2101 ),
 ( #5494, #8878, #412 ) ),
 .UNSPECIFIED., .F., .F., .T. ) 
 B_SPLINE_SURFACE_WITH_KNOTS ( ( 4, 2, 4 ),
 ( 3, 3 ),
 ( 0.02032853247518125531, 0.02278863295364820865, 0.02524873343211516200 ),
 ( 0.000000000000000000, 1.000000000000000000 ),
 .UNSPECIFIED. ) 
 GEOMETRIC_REPRESENTATION_ITEM ( )  RATIONAL_B_SPLINE_SURFACE ( (
 ( 1.000000000000000000, 0.8047781615896836271, 1.000000000000000000),
 ( 1.000000000000000000, 0.8123767586289967202, 1.000000000000000000),
 ( 1.000000000000000000, 0.8190662415563443322, 1.000000000000000000),
 ( 1.000000000000000000, 0.8192361015669982205, 1.000000000000000000),
 ( 1.000000000000000000, 0.8126135807103181952, 1.000000000000000000),
 ( 1.000000000000000000, 0.8047712338318587788, 1.000000000000000000) ) ) 
 REPRESENTATION_ITEM ( '' )  SURFACE ( )  );
#6171 = VERTEX_POINT ( 'NONE', #9739 ) ;
#6172 = CIRCLE ( 'NONE', #7948, 1.535500000000000087 ) ;
#6173 = CARTESIAN_POINT ( 'NONE',  ( 1.720978244806805169, 31.81455566112594013, 13.75219158473306535 ) ) ;
#6174 = ORIENTED_EDGE ( 'NONE', *, *, #7713, .T. ) ;
#6175 = CARTESIAN_POINT ( 'NONE',  ( 18.81331750051067075, 21.67874213615617762, 12.94889058896551326 ) ) ;
#6176 = SHAPE_REPRESENTATION_RELATIONSHIP ( 'NONE' , 'NONE' ,  #3016, #2840 ) ;
#6177 = CARTESIAN_POINT ( 'NONE',  ( 2.121320343559645494, 32.12132034355964549, 13.50000000000000355 ) ) ;
#6178 = PRESENTATION_LAYER_ASSIGNMENT (  '', '', ( #10265 ) ) ;
#6179 =( GEOMETRIC_REPRESENTATION_CONTEXT ( 3 ) GLOBAL_UNCERTAINTY_ASSIGNED_CONTEXT ( ( #6983 ) ) GLOBAL_UNIT_ASSIGNED_CONTEXT ( ( #3841, #1287, #9836 ) ) REPRESENTATION_CONTEXT ( 'NONE', 'WORKASPACE' ) );
#6180 = CARTESIAN_POINT ( 'NONE',  ( 29.50000000000000711, 1.387778780781445676E-14, 17.49999999999999645 ) ) ;
#6181 = CARTESIAN_POINT ( 'NONE',  ( -24.35964822603314772, 53.16041666571062763, -4.064049460664953983 ) ) ;
#6182 = AXIS2_PLACEMENT_3D ( 'NONE', #2596, #8868, #10531 ) ;
#6183 = DIRECTION ( 'NONE',  ( 1.000000000000000000, 6.098637220230963674E-17, 1.156482317317871478E-16 ) ) ;
#6184 = CARTESIAN_POINT ( 'NONE',  ( 34.99999999999987210, -3.999999999999989786, -2.850000000000004530 ) ) ;
#6185 = VERTEX_POINT ( 'NONE', #9624 ) ;
#6186 = VERTEX_POINT ( 'NONE', #9789 ) ;
#6187 = DIRECTION ( 'NONE',  ( 0.000000000000000000, 0.000000000000000000, -1.000000000000000000 ) ) ;
#6188 = CARTESIAN_POINT ( 'NONE',  ( 34.94281041931228771, 2.000000000000002220, 2.500000000000000000 ) ) ;
#6189 = EDGE_CURVE ( 'NONE', #6838, #652, #7068, .T. ) ;
#6190 = FACE_OUTER_BOUND ( 'NONE', #4749, .T. ) ;
#6191 = CARTESIAN_POINT ( 'NONE',  ( -21.21106610644865498, 16.50000000000026290, -9.500000000000000000 ) ) ;
#6192 = CARTESIAN_POINT ( 'NONE',  ( 0.000000000000000000, 0.000000000000000000, 0.000000000000000000 ) ) ;
#6193 = CARTESIAN_POINT ( 'NONE',  ( 3.903127820947815962E-15, 26.49999999999999289, 14.28125000000000355 ) ) ;
#6194 = DIRECTION ( 'NONE',  ( 0.000000000000000000, 0.000000000000000000, -1.000000000000000000 ) ) ;
#6195 = ORIENTED_EDGE ( 'NONE', *, *, #8047, .T. ) ;
#6196 = DIRECTION ( 'NONE',  ( 0.000000000000000000, -1.000000000000000000, 0.000000000000000000 ) ) ;
#6197 = CARTESIAN_POINT ( 'NONE',  ( 1.101703131577913553, 32.47259180932605460, 14.57593341526694175 ) ) ;
#6198 = CARTESIAN_POINT ( 'NONE',  ( -1.767766952966375094, 31.76776695296636888, 13.81250000000000355 ) ) ;
#6199 = UNCERTAINTY_MEASURE_WITH_UNIT (LENGTH_MEASURE( 1.000000000000000082E-05 ), #3838, 'distance_accuracy_value', 'NONE');
#6200 = EDGE_CURVE ( 'NONE', #4976, #4616, #2813, .T. ) ;
#6201 = CARTESIAN_POINT ( 'NONE',  ( 3.469446951953614189E-15, -1.040834085586084257E-14, 2.500000000000000000 ) ) ;
#6202 = CARTESIAN_POINT ( 'NONE',  ( -1.882954241746308865E-15, 2.859595677584315432, -2.047034997319608252 ) ) ;
#6203 = EDGE_CURVE ( 'NONE', #609, #3529, #7126, .T. ) ;
#6204 = CARTESIAN_POINT ( 'NONE',  ( -25.98076211353311393, 53.21874999904395054, -3.128098921329806714 ) ) ;
#6205 = CARTESIAN_POINT ( 'NONE',  ( 29.49999999999999289, -9.999999999999998224, 15.50000000000000711 ) ) ;
#6206 = DIRECTION ( 'NONE',  ( 0.000000000000000000, 0.000000000000000000, 1.000000000000000000 ) ) ;
#6207 = ORIENTED_EDGE ( 'NONE', *, *, #2832, .F. ) ;
#6208 = ORIENTED_EDGE ( 'NONE', *, *, #905, .T. ) ;
#6209 = CARTESIAN_POINT ( 'NONE',  ( -25.44486372867087454, 50.95623925897108109, -7.000000000000073719 ) ) ;
#6210 = ADVANCED_FACE ( 'NONE', ( #448, #3848 ), #7233, .T. ) ;
#6211 = DIRECTION ( 'NONE',  ( -1.000000000000000000, -6.098637220230963674E-17, 0.000000000000000000 ) ) ;
#6212 = DIRECTION ( 'NONE',  ( -1.000000000000000000, 0.000000000000000000, 6.123233995736766036E-17 ) ) ;
#6213 = ORIENTED_EDGE ( 'NONE', *, *, #4393, .F. ) ;
#6214 = ADVANCED_FACE ( 'NONE', ( #232 ), #3628, .T. ) ;
#6215 = CARTESIAN_POINT ( 'NONE',  ( 0.000000000000000000, 0.000000000000000000, 0.000000000000000000 ) ) ;
#6216 = CARTESIAN_POINT ( 'NONE',  ( 0.6666666666666689611, 4.233901974057261874, -3.300726591567082480 ) ) ;
#6217 = CARTESIAN_POINT ( 'NONE',  ( 18.23429108146684641, 17.05446421968790460, 11.03858925989339390 ) ) ;
#6218 = DIRECTION ( 'NONE',  ( 1.000000000000000000, 6.098637220230963674E-17, 1.156482317317871478E-16 ) ) ;
#6219 = CARTESIAN_POINT ( 'NONE',  ( -25.98076211353311393, 52.51874999904395480, -3.128098921329806714 ) ) ;
#6220 = CARTESIAN_POINT ( 'NONE',  ( 3.199999999999999734, -3.031088913245550298, -1.749999999999972911 ) ) ;
#6221 = ORIENTED_EDGE ( 'NONE', *, *, #2254, .T. ) ;
#6222 = CARTESIAN_POINT ( 'NONE',  ( 29.49999999999999289, 14.99999999999984546, 2.500000000000000000 ) ) ;
#6223 = ORIENTED_EDGE ( 'NONE', *, *, #5550, .F. ) ;
#6224 = CARTESIAN_POINT ( 'NONE',  ( -0.9693646802875608426, 27.47259180932603684, 13.20531658473306713 ) ) ;
#6225 = ORIENTED_EDGE ( 'NONE', *, *, #10443, .F. ) ;
#6226 = CARTESIAN_POINT ( 'NONE',  ( 16.50280774463635680, 17.03272616129868666, 12.11810441208646338 ) ) ;
#6227 = DIRECTION ( 'NONE',  ( 0.000000000000000000, -0.000000000000000000, -1.000000000000000000 ) ) ;
#6228 = CARTESIAN_POINT ( 'NONE',  ( 16.54959645279592451, 16.98593745313911896, 13.11591282735340336 ) ) ;
#6229 = CARTESIAN_POINT ( 'NONE',  ( -24.35964822603314417, 54.61874999904395622, -5.000000000000103029 ) ) ;
#6230 = VECTOR ( 'NONE', #8027, 1000.000000000000000 ) ;
#6231 =( BOUNDED_SURFACE ( )  B_SPLINE_SURFACE ( 3, 2, ( 
 ( #6920, #9363, #4313 ),
 ( #6029, #76, #1926 ),
 ( #10309, #5363, #5258 ),
 ( #7868, #4434, #8746 ),
 ( #9469, #7644, #138 ),
 ( #5313, #2654, #9578 ) ),
 .UNSPECIFIED., .F., .F., .F. ) 
 B_SPLINE_SURFACE_WITH_KNOTS ( ( 4, 2, 4 ),
 ( 3, 3 ),
 ( 0.02032853247518126225, 0.02278863295364821212, 0.02524873343211516200 ),
 ( 0.000000000000000000, 1.000000000000000000 ),
 .UNSPECIFIED. ) 
 GEOMETRIC_REPRESENTATION_ITEM ( )  RATIONAL_B_SPLINE_SURFACE ( (
 ( 1.000000000000000000, 0.8047781615896835161, 1.000000000000000000),
 ( 1.000000000000000000, 0.8123767586291043008, 1.000000000000000000),
 ( 1.000000000000000000, 0.8190662415562011134, 1.000000000000000000),
 ( 1.000000000000000000, 0.8192361015671398849, 1.000000000000000000),
 ( 1.000000000000000000, 0.8126135807102121689, 1.000000000000000000),
 ( 1.000000000000000000, 0.8047712338318585568, 1.000000000000000000) ) ) 
 REPRESENTATION_ITEM ( '' )  SURFACE ( )  );
#6232 = DIRECTION ( 'NONE',  ( 6.098637220230963674E-17, -1.000000000000000000, 0.000000000000000000 ) ) ;
#6233 = CARTESIAN_POINT ( 'NONE',  ( -24.98076211353312814, 50.22916666475470038, -6.732050807568954909 ) ) ;
#6234 = DIRECTION ( 'NONE',  ( 0.000000000000000000, 0.000000000000000000, 1.000000000000000000 ) ) ;
#6235 = ORIENTED_EDGE ( 'NONE', *, *, #5214, .T. ) ;
#6236 = LINE ( 'NONE', #5412, #3487 ) ;
#6237 = CARTESIAN_POINT ( 'NONE',  ( -25.98076211353311393, 49.49999999999986500, -5.000000000000103029 ) ) ;
#6238 = FACE_OUTER_BOUND ( 'NONE', #7070, .T. ) ;
#6239 = CARTESIAN_POINT ( 'NONE',  ( 0.000000000000000000, 0.000000000000000000, 0.000000000000000000 ) ) ;
#6240 = LINE ( 'NONE', #348, #674 ) ;
#6241 = DIRECTION ( 'NONE',  ( -1.000000000000000000, 0.000000000000000000, 0.000000000000000000 ) ) ;
#6242 = DIRECTION ( 'NONE',  ( -1.000000000000000000, -6.098637220230964906E-17, 0.000000000000000000 ) ) ;
#6243 = CARTESIAN_POINT ( 'NONE',  ( 2.428085025993357071, 27.47833755768751374, 16.68530841526694175 ) ) ;
#6244 = FACE_OUTER_BOUND ( 'NONE', #5114, .T. ) ;
#6245 = EDGE_LOOP ( 'NONE', ( #5784, #6158 ) ) ;
#6246 = SURFACE_STYLE_FILL_AREA ( #2146 ) ;
#6247 = CARTESIAN_POINT ( 'NONE',  ( 2.500000000000007550, 31.03553390593274486, 15.92187500000000178 ) ) ;
#6248 = CARTESIAN_POINT ( 'NONE',  ( 1.035533905932743970, 27.49999999999999289, 14.35937500000000711 ) ) ;
#6249 = VECTOR ( 'NONE', #10266, 1000.000000000000000 ) ;
#6250 = CARTESIAN_POINT ( 'NONE',  ( 22.29575558078030895, 19.24694448270711788, 12.00579112326941988 ) ) ;
#6251 = CYLINDRICAL_SURFACE ( 'NONE', #9118, 2.149999999999992362 ) ;
#6252 = CARTESIAN_POINT ( 'NONE',  ( 2.500000000000000000, -1.178949249685213863, 2.042000000000002924 ) ) ;
#6253 = CARTESIAN_POINT ( 'NONE',  ( -2.712762565639006418, 3.052587955997511759, -3.430618716626627318 ) ) ;
#6254 = CARTESIAN_POINT ( 'NONE',  ( -27.60187600103308370, 51.64374999904394770, -5.000000000000103029 ) ) ;
#6255 = CARTESIAN_POINT ( 'NONE',  ( 0.3126073911696528040, 2.020725942163738686, 3.499999999999999556 ) ) ;
#6256 = DIRECTION ( 'NONE',  ( 0.000000000000000000, 0.000000000000000000, -1.000000000000000000 ) ) ;
#6257 = ORIENTED_EDGE ( 'NONE', *, *, #9452, .F. ) ;
#6258 = VERTEX_POINT ( 'NONE', #5729 ) ;
#6259 = CARTESIAN_POINT ( 'NONE',  ( -25.98076211353324894, 13.49999999999941913, -5.000000000000000000 ) ) ;
#6260 = DIRECTION ( 'NONE',  ( -2.775557561562891351E-17, -1.000000000000000000, 8.326672684688671588E-17 ) ) ;
#6261 = ADVANCED_BREP_SHAPE_REPRESENTATION ( '', ( #9072, #308 ), #7601 ) ;
#6262 = ORIENTED_EDGE ( 'NONE', *, *, #3495, .T. ) ;
#6263 = CARTESIAN_POINT ( 'NONE',  ( 29.50000000000000711, -3.999999999999989786, 12.14999999999999147 ) ) ;
#6264 = CARTESIAN_POINT ( 'NONE',  ( -25.17020516978313083, 50.53541666571062052, -6.403925809002825709 ) ) ;
#6265 = CARTESIAN_POINT ( 'NONE',  ( 23.98154255942039370, 19.66242269470938453, 10.95195840513859586 ) ) ;
#6266 = EDGE_CURVE ( 'NONE', #1508, #8762, #4846, .T. ) ;
#6267 = ORIENTED_EDGE ( 'NONE', *, *, #8656, .F. ) ;
#6268 = EDGE_CURVE ( 'NONE', #3160, #5721, #2390, .T. ) ;
#6269 = CARTESIAN_POINT ( 'NONE',  ( -27.60187600103308370, 54.44374999904394485, -5.000000000000103029 ) ) ;
#6270 = ORIENTED_EDGE ( 'NONE', *, *, #8301, .T. ) ;
#6271 = LINE ( 'NONE', #10457, #7230 ) ;
#6272 = VERTEX_POINT ( 'NONE', #6555 ) ;
#6273 = CARTESIAN_POINT ( 'NONE',  ( -2.472591809326046608, 28.89829686842208289, 13.04906658473306891 ) ) ;
#6274 = ORIENTED_EDGE ( 'NONE', *, *, #1924, .F. ) ;
#6275 = CARTESIAN_POINT ( 'NONE',  ( 18.76105380172462844, 21.09515122317004909, 11.95042449705224819 ) ) ;
#6276 =( REPRESENTATION_RELATIONSHIP ('NONE','NONE', #7540, #1223 ) REPRESENTATION_RELATIONSHIP_WITH_TRANSFORMATION ( #4615 )SHAPE_REPRESENTATION_RELATIONSHIP( ) );
#6277 = CIRCLE ( 'NONE', #8940, 3.000000000000000000 ) ;
#6278 = CARTESIAN_POINT ( 'NONE',  ( -2.649999999999991029, 30.00000000000000000, 2.500000000000000000 ) ) ;
#6279 = CARTESIAN_POINT ( 'NONE',  ( 22.32737213215407479, 19.20149278331202325, 13.00425721518307576 ) ) ;
#6280 = EDGE_CURVE ( 'NONE', #4274, #6817, #6462, .T. ) ;
#6281 = CARTESIAN_POINT ( 'NONE',  ( -26.79131905728310059, 53.68541666571061910, -3.596074190997381237 ) ) ;
#6282 = FACE_OUTER_BOUND ( 'NONE', #9073, .T. ) ;
#6283 = FACE_OUTER_BOUND ( 'NONE', #449, .T. ) ;
#6284 = LINE ( 'NONE', #5465, #2430 ) ;
#6285 = ORIENTED_EDGE ( 'NONE', *, *, #2110, .T. ) ;
#6286 = CIRCLE ( 'NONE', #9300, 3.499999999999999556 ) ;
#6287 = ORIENTED_EDGE ( 'NONE', *, *, #8168, .T. ) ;
#6288 = EDGE_CURVE ( 'NONE', #6109, #1566, #4304, .T. ) ;
#6289 = CARTESIAN_POINT ( 'NONE',  ( 19.85760542366876535, 20.31250532737884384, 12.00579112326941988 ) ) ;
#6290 = DIRECTION ( 'NONE',  ( 0.000000000000000000, 0.000000000000000000, 1.000000000000000000 ) ) ;
#6291 = CARTESIAN_POINT ( 'NONE',  ( -25.98076211353311393, 53.43749999808803608, -3.000000000000132339 ) ) ;
#6292 = VECTOR ( 'NONE', #210, 1000.000000000000000 ) ;
#6293 = CARTESIAN_POINT ( 'NONE',  ( 29.50000000000000711, 2.000000000000001776, -5.500000000000000000 ) ) ;
#6294 = CYLINDRICAL_SURFACE ( 'NONE', #10627, 4.500000000000000000 ) ;
#6295 = CARTESIAN_POINT ( 'NONE',  ( 3.199999999999987743, 2.859595677584378937, 2.047034997319559846 ) ) ;
#6296 = DIRECTION ( 'NONE',  ( -0.000000000000000000, -0.000000000000000000, -1.000000000000000000 ) ) ;
#6297 = AXIS2_PLACEMENT_3D ( 'NONE', #8498, #935, #7670 ) ;
#6298 = DIRECTION ( 'NONE',  ( 0.000000000000000000, 0.000000000000000000, -1.000000000000000000 ) ) ;
#6299 = CARTESIAN_POINT ( 'NONE',  ( 1.449747468305836673, 26.49999999999999289, 14.35937500000000711 ) ) ;
#6300 = FACE_OUTER_BOUND ( 'NONE', #8622, .T. ) ;
#6301 = EDGE_CURVE ( 'NONE', #233, #1715, #7447, .T. ) ;
#6302 = VERTEX_POINT ( 'NONE', #1561 ) ;
#6303 = DIRECTION ( 'NONE',  ( -0.8660254037844398178, -0.4999999999999978351, 0.000000000000000000 ) ) ;
#6304 = B_SPLINE_CURVE_WITH_KNOTS ( 'NONE', 3,
 ( #309, #9477, #2828, #7141, #2035, #1873 ),
 .UNSPECIFIED., .F., .F.,
 ( 4, 2, 4 ),
 ( 0.002452478801916361129, 0.003676905084148001344, 0.004901331366379641126 ),
 .UNSPECIFIED. ) ;
#6305 = AXIS2_PLACEMENT_3D ( 'NONE', #9338, #8619, #828 ) ;
#6306 = VECTOR ( 'NONE', #398, 999.9999999999998863 ) ;
#6307 = CARTESIAN_POINT ( 'NONE',  ( -2.385244779468109755E-15, 32.50000000000000711, 16.15625000000000355 ) ) ;
#6308 = CARTESIAN_POINT ( 'NONE',  ( 1.035533905932737975, 32.50000000000000711, 13.57812500000000178 ) ) ;
#6309 = VECTOR ( 'NONE', #738, 1000.000000000000000 ) ;
#6310 = CARTESIAN_POINT ( 'NONE',  ( 19.95755123817951215, 17.62047157401400810, 12.00579112326941988 ) ) ;
#6311 = CARTESIAN_POINT ( 'NONE',  ( 34.99999999999999289, -3.999999999999993339, -7.149999999999983480 ) ) ;
#6312 = CARTESIAN_POINT ( 'NONE',  ( -24.98076211353313170, 52.88333333333319786, -3.267949192431250705 ) ) ;
#6313 = AXIS2_PLACEMENT_3D ( 'NONE', #2513, #5957, #895 ) ;
#6314 = CARTESIAN_POINT ( 'NONE',  ( -4.211140560182196957, -2.431303136016552013, -3.745885042887436178 ) ) ;
#6315 = CARTESIAN_POINT ( 'NONE',  ( -24.35964822603314417, 51.99374999904394201, -5.000000000000103029 ) ) ;
#6316 = DIRECTION ( 'NONE',  ( 0.000000000000000000, 0.000000000000000000, 1.000000000000000000 ) ) ;
#6317 = CARTESIAN_POINT ( 'NONE',  ( 2.500000000000000000, 2.357898499370433054, -1.951563910473907981E-15 ) ) ;
#6318 = AXIS2_PLACEMENT_3D ( 'NONE', #5791, #10077, #7514 ) ;
#6319 = ORIENTED_EDGE ( 'NONE', *, *, #192, .T. ) ;
#6320 = DIRECTION ( 'NONE',  ( 0.000000000000000000, 1.000000000000000000, 0.000000000000000000 ) ) ;
#6321 = ITEM_DEFINED_TRANSFORMATION ( 'NONE', 'NONE', #4400,  #308 ) ;
#6322 = ORIENTED_EDGE ( 'NONE', *, *, #9496, .T. ) ;
#6323 = LINE ( 'NONE', #8833, #8613 ) ;
#6324 = CARTESIAN_POINT ( 'NONE',  ( 29.49999999999999289, 5.000000000000000888, 5.500000000000000000 ) ) ;
#6325 = EDGE_CURVE ( 'NONE', #9151, #3779, #3950, .T. ) ;
#6326 = CARTESIAN_POINT ( 'NONE',  ( 22.93674656822681612, 23.24041807713223307, 10.95195840513859231 ) ) ;
#6327 = EDGE_LOOP ( 'NONE', ( #3208, #6629, #3658, #5291 ) ) ;
#6328 = CARTESIAN_POINT ( 'NONE',  ( -25.17020516978313083, 54.91041666571061342, -6.403925809002825709 ) ) ;
#6329 = ORIENTED_EDGE ( 'NONE', *, *, #90, .F. ) ;
#6330 = FACE_OUTER_BOUND ( 'NONE', #419, .T. ) ;
#6331 = VERTEX_POINT ( 'NONE', #4065 ) ;
#6332 = CARTESIAN_POINT ( 'NONE',  ( 1.035533905932743970, 27.49999999999999289, 14.35937500000000711 ) ) ;
#6333 = VERTEX_POINT ( 'NONE', #7334 ) ;
#6335 = CARTESIAN_POINT ( 'NONE',  ( 21.01569960522067504, 17.20769859423666048, 10.95195840513859231 ) ) ;
#6334 = CIRCLE ( 'NONE', #9167, 3.249999999999998224 ) ;
#6336 = PRODUCT_DEFINITION_FORMATION_WITH_SPECIFIED_SOURCE ( 'ANY', '', #3417, .NOT_KNOWN. ) ;
#6337 = SURFACE_STYLE_FILL_AREA ( #336 ) ;
#6338 = EDGE_CURVE ( 'NONE', #7545, #7348, #2456, .T. ) ;
#6339 = DIRECTION ( 'NONE',  ( 1.000000000000000000, 0.000000000000000000, 0.000000000000000000 ) ) ;
#6340 = EDGE_CURVE ( 'NONE', #6740, #5854, #3788, .T. ) ;
#6341 = CARTESIAN_POINT ( 'NONE',  ( 22.86397682584157565, 19.61629903322988966, 13.00425721518307753 ) ) ;
#6342 = CARTESIAN_POINT ( 'NONE',  ( 2.500000000000000000, 0.000000000000000000, 0.000000000000000000 ) ) ;
#6343 = AXIS2_PLACEMENT_3D ( 'NONE', #6070, #8633, #4476 ) ;
#6344 = AXIS2_PLACEMENT_3D ( 'NONE', #2448, #9387, #7617 ) ;
#6345 = DIRECTION ( 'NONE',  ( -1.000000000000000000, -6.098637220230964906E-17, 0.000000000000000000 ) ) ;
#6346 = CARTESIAN_POINT ( 'NONE',  ( -23.98076211353314235, 52.97083333142136752, -6.154700538379337615 ) ) ;
#6347 = ORIENTED_EDGE ( 'NONE', *, *, #9398, .T. ) ;
#6348 = ORIENTED_EDGE ( 'NONE', *, *, #2201, .T. ) ;
#6349 = CARTESIAN_POINT ( 'NONE',  ( 23.13231036272843966, 20.08340223762181154, 12.00579112326941988 ) ) ;
#6350 = ADVANCED_FACE ( 'NONE', ( #8334 ), #6498, .F. ) ;
#6351 = DIRECTION ( 'NONE',  ( 1.000000000000000000, 0.000000000000000000, 0.000000000000000000 ) ) ;
#6352 = VECTOR ( 'NONE', #1108, 1000.000000000000000 ) ;
#6353 =( GEOMETRIC_REPRESENTATION_CONTEXT ( 3 ) GLOBAL_UNCERTAINTY_ASSIGNED_CONTEXT ( ( #9242 ) ) GLOBAL_UNIT_ASSIGNED_CONTEXT ( ( #2, #9731, #10462 ) ) REPRESENTATION_CONTEXT ( 'NONE', 'WORKASPACE' ) );
#6354 = DIRECTION ( 'NONE',  ( 0.000000000000000000, 0.000000000000000000, -1.000000000000000000 ) ) ;
#6355 = CARTESIAN_POINT ( 'NONE',  ( 3.333333333333335702, -2.694301256218268215, -3.300726591567084256 ) ) ;
#6356 = CYLINDRICAL_SURFACE ( 'NONE', #8718, 1.649999999999994360 ) ;
#6357 = FACE_OUTER_BOUND ( 'NONE', #4935, .T. ) ;
#6358 = CARTESIAN_POINT ( 'NONE',  ( 23.89484671925281845, 19.39402032390267649, 11.95042449705224819 ) ) ;
#6359 = ADVANCED_FACE ( 'NONE', ( #4906 ), #7282, .T. ) ;
#6360 = EDGE_CURVE ( 'NONE', #6057, #8126, #607, .T. ) ;
#6361 = EDGE_CURVE ( 'NONE', #1944, #1390, #9012, .T. ) ;
#6362 = CARTESIAN_POINT ( 'NONE',  ( -5.076455387921347651, 24.47916666666666075, 2.499999999999999112 ) ) ;
#6363 = CARTESIAN_POINT ( 'NONE',  ( 3.500000000000007994, 28.55025253169416644, 15.76562500000000178 ) ) ;
#6364 = CARTESIAN_POINT ( 'NONE',  ( 4.750000000000000888, 0.000000000000000000, 0.000000000000000000 ) ) ;
#6365 = ORIENTED_EDGE ( 'NONE', *, *, #1059, .F. ) ;
#6366 = PRESENTATION_LAYER_ASSIGNMENT (  '', '', ( #4953 ) ) ;
#6367 = CARTESIAN_POINT ( 'NONE',  ( -3.505208318772512488, 29.79067687212226545, 17.48140433884295319 ) ) ;
#6368 = AXIS2_PLACEMENT_3D ( 'NONE', #6660, #8446, #6451 ) ;
#6369 = CARTESIAN_POINT ( 'NONE',  ( -0.06616922564517119243, 26.49999999999999289, 15.27905841526694175 ) ) ;
#6370 = FACE_OUTER_BOUND ( 'NONE', #7902, .T. ) ;
#6371 = DIRECTION ( 'NONE',  ( -1.000000000000000000, -6.098637220230963674E-17, 0.000000000000000000 ) ) ;
#6372 = CARTESIAN_POINT ( 'NONE',  ( -24.98076211353313170, 53.49583333142136610, -3.267949192431250705 ) ) ;
#6373 = CARTESIAN_POINT ( 'NONE',  ( 0.000000000000000000, 1.773042676681340524, -2.059984127722458425E-15 ) ) ;
#6374 = CARTESIAN_POINT ( 'NONE',  ( -24.35964822603314772, 52.75208333237727487, -5.935950539335252074 ) ) ;
#6375 = DIRECTION ( 'NONE',  ( -1.000000000000000000, -0.000000000000000000, -0.000000000000000000 ) ) ;
#6376 = CARTESIAN_POINT ( 'NONE',  ( -4.235886605889389145, -2.417314728048544303, -3.751161874094020909 ) ) ;
#6377 = ORIENTED_EDGE ( 'NONE', *, *, #6483, .T. ) ;
#6378 = CARTESIAN_POINT ( 'NONE',  ( -2.000000000000007550, -3.464101615137749945, 0.000000000000000000 ) ) ;
#6379 = EDGE_CURVE ( 'NONE', #6934, #3459, #10002, .T. ) ;
#6380 = ADVANCED_FACE ( 'NONE', ( #6665 ), #10064, .F. ) ;
#6381 = ORIENTED_EDGE ( 'NONE', *, *, #4243, .T. ) ;
#6382 = CYLINDRICAL_SURFACE ( 'NONE', #4161, 1.999999999999971356 ) ;
#6383 = CARTESIAN_POINT ( 'NONE',  ( -24.35964822603314772, 51.06041666571061910, -4.064049460664953983 ) ) ;
#6384 = CARTESIAN_POINT ( 'NONE',  ( 17.08513846059531005, 17.86460900771146143, 11.12760988119559258 ) ) ;
#6385 = ORIENTED_EDGE ( 'NONE', *, *, #8047, .F. ) ;
#6386 = CARTESIAN_POINT ( 'NONE',  ( 34.74418829745650328, 4.228279689541292186, 2.594445730714923126 ) ) ;
#6387 = EDGE_LOOP ( 'NONE', ( #1274, #5867, #3663, #3699 ) ) ;
#6388 = DIRECTION ( 'NONE',  ( 0.000000000000000000, 0.000000000000000000, -1.000000000000000000 ) ) ;
#6389 = ORIENTED_EDGE ( 'NONE', *, *, #9265, .F. ) ;
#6390 = CARTESIAN_POINT ( 'NONE',  ( 1.720978244806805169, 31.81455566112594013, 15.00219158473306535 ) ) ;
#6391 = EDGE_LOOP ( 'NONE', ( #7884, #4889, #5397, #3631, #1317, #1545, #5949, #2837, #10412, #10819, #7270, #334, #577, #10739 ) ) ;
#6392 = CARTESIAN_POINT ( 'NONE',  ( 16.14406960823794179, 17.39146429769401081, 11.14955153432450530 ) ) ;
#6393 = CARTESIAN_POINT ( 'NONE',  ( 3.436319922986518449, -2.634841920959471562, -3.531542292954761741 ) ) ;
#6394 = CARTESIAN_POINT ( 'NONE',  ( 20.19688095354152324, 19.67517542290917731, 13.00425721518307753 ) ) ;
#6395 = CARTESIAN_POINT ( 'NONE',  ( -23.98076211353314235, 52.21249999808803466, -5.000000000000103029 ) ) ;
#6396 = PRODUCT_DEFINITION ( 'UNKNOWN', '', #8462, #4907 ) ;
#6397 = CARTESIAN_POINT ( 'NONE',  ( -26.98076211353309972, 53.23333333333319217, -6.732050807568954909 ) ) ;
#6398 = ORIENTED_EDGE ( 'NONE', *, *, #635, .F. ) ;
#6399 = ORIENTED_EDGE ( 'NONE', *, *, #4243, .F. ) ;
#6400 = CARTESIAN_POINT ( 'NONE',  ( 17.83714238635922911, 17.16560587574106123, 13.06440897074317853 ) ) ;
#6401 = CARTESIAN_POINT ( 'NONE',  ( -27.98076211353308551, 49.79166666666652930, -6.154700538379338504 ) ) ;
#6402 = SHAPE_REPRESENTATION ( 'hex flange nut gradea_iso_ISO - 4161 - M5 - N', ( #308 ), #6687 ) ;
#6403 = DIRECTION ( 'NONE',  ( 0.000000000000000000, 0.000000000000000000, -1.000000000000000000 ) ) ;
#6404 = CARTESIAN_POINT ( 'NONE',  ( 4.000000000000000000, 0.7924765000094659007, -0.05906175389889852662 ) ) ;
#6405 = CARTESIAN_POINT ( 'NONE',  ( 3.500000000000005329, 30.00000000000000000, 15.84375000000000355 ) ) ;
#6406 = DIRECTION ( 'NONE',  ( -4.312387734421983138E-17, 0.7071067811865463515, 0.7071067811865487940 ) ) ;
#6407 = EDGE_CURVE ( 'NONE', #6258, #4348, #9542, .T. ) ;
#6408 = ORIENTED_EDGE ( 'NONE', *, *, #8807, .F. ) ;
#6409 = EDGE_CURVE ( 'NONE', #276, #2646, #9393, .T. ) ;
#6410 = CIRCLE ( 'NONE', #2512, 3.369999999999997886 ) ;
#6411 = CARTESIAN_POINT ( 'NONE',  ( 0.06616922564517314920, 33.50000000000000000, 15.90405841526694175 ) ) ;
#6412 = DIRECTION ( 'NONE',  ( 1.000000000000000000, 0.000000000000000000, 0.000000000000000000 ) ) ;
#6413 = LINE ( 'NONE', #3246, #1859 ) ;
#6414 = DIRECTION ( 'NONE',  ( 0.000000000000000000, 1.000000000000000000, -1.345283343056720273E-15 ) ) ;
#6415 = CARTESIAN_POINT ( 'NONE',  ( -25.98076211353311393, 51.77499999999986358, -7.000000000000072831 ) ) ;
#6416 = CARTESIAN_POINT ( 'NONE',  ( -27.60187600103308014, 53.68541666571061199, -5.935950539335252074 ) ) ;
#6417 = DIRECTION ( 'NONE',  ( 0.000000000000000000, 0.000000000000000000, 1.000000000000000000 ) ) ;
#6418 = CARTESIAN_POINT ( 'NONE',  ( 0.02511973781850649831, -4.877415612947427981, -3.751298745799844792 ) ) ;
#6419 = B_SPLINE_CURVE_WITH_KNOTS ( 'NONE', 3,
 ( #5924, #9311, #9704, #10596, #2039, #9645 ),
 .UNSPECIFIED., .F., .F.,
 ( 4, 2, 4 ),
 ( 0.003358874760055550156, 0.004541967308452096383, 0.005725059856848641743 ),
 .UNSPECIFIED. ) ;
#6420 = ORIENTED_EDGE ( 'NONE', *, *, #9626, .T. ) ;
#6421 = CARTESIAN_POINT ( 'NONE',  ( -23.98076211353314235, 54.37083333142137320, -6.154700538379337615 ) ) ;
#6422 = AXIS2_PLACEMENT_3D ( 'NONE', #2624, #6945, #4343 ) ;
#6423 = CARTESIAN_POINT ( 'NONE',  ( 34.99999999999987210, -7.999999999999983125, 17.49999999999999645 ) ) ;
#6424 = VERTEX_POINT ( 'NONE', #2682 ) ;
#6425 = CARTESIAN_POINT ( 'NONE',  ( -25.17020516978313083, 50.71041666571061057, -6.403925809002825709 ) ) ;
#6426 = CARTESIAN_POINT ( 'NONE',  ( 4.200000000000001954, 0.000000000000000000, 0.000000000000000000 ) ) ;
#6427 = VECTOR ( 'NONE', #3614, 1000.000000000000000 ) ;
#6428 = CARTESIAN_POINT ( 'NONE',  ( 17.45361707773674809, 17.49611573659335662, 12.09524845743996657 ) ) ;
#6429 = VERTEX_POINT ( 'NONE', #6058 ) ;
#6430 = CARTESIAN_POINT ( 'NONE',  ( 34.86952523334974785, 3.022518564432433497, 3.235504471074991617 ) ) ;
#6432 = ORIENTED_EDGE ( 'NONE', *, *, #5699, .F. ) ;
#6431 = ADVANCED_FACE ( 'NONE', ( #10288 ), #6513, .F. ) ;
#6433 = DIRECTION ( 'NONE',  ( -1.000000000000000000, 0.000000000000000000, 0.000000000000000000 ) ) ;
#6434 = EDGE_LOOP ( 'NONE', ( #9157, #3753, #5077, #9262, #6556 ) ) ;
#6435 = CARTESIAN_POINT ( 'NONE',  ( 27.50000000000001066, -3.999999999999983569, 10.00000000000000888 ) ) ;
#6436 = FILL_AREA_STYLE_COLOUR ( '', #6523 ) ;
#6437 = ORIENTED_EDGE ( 'NONE', *, *, #9192, .F. ) ;
#6438 = CARTESIAN_POINT ( 'NONE',  ( 16.85117638942448082, 18.09857107888056760, 11.14955153432450530 ) ) ;
#6439 = DIRECTION ( 'NONE',  ( 1.000000000000000000, -0.000000000000000000, -0.000000000000000000 ) ) ;
#6440 = CARTESIAN_POINT ( 'NONE',  ( 16.23764702455707720, 17.29788688137487185, 13.14516836485838169 ) ) ;
#6441 = CARTESIAN_POINT ( 'NONE',  ( -25.98076211353311393, 51.68749999808803608, -7.309401076758571314 ) ) ;
#6442 = PLANE ( 'NONE',  #10730 ) ;
#6443 = CARTESIAN_POINT ( 'NONE',  ( -27.98076211353308551, 51.10416666475469327, -6.154700538379338504 ) ) ;
#6444 = VERTEX_POINT ( 'NONE', #6903 ) ;
#6445 = ORIENTED_EDGE ( 'NONE', *, *, #2398, .T. ) ;
#6446 = CARTESIAN_POINT ( 'NONE',  ( 22.63806431670481700, 19.48506897666907989, 12.00579112326951758 ) ) ;
#6447 = CARTESIAN_POINT ( 'NONE',  ( 3.200000000000000178, 2.020725942163657862, -3.499999999999999556 ) ) ;
#6448 = CARTESIAN_POINT ( 'NONE',  ( -3.264650091097280831E-13, -4.796980096169642493, -3.721999068284424617 ) ) ;
#6449 = FACE_OUTER_BOUND ( 'NONE', #7463, .T. ) ;
#6450 = ADVANCED_FACE ( 'NONE', ( #1841 ), #9340, .F. ) ;
#6451 = DIRECTION ( 'NONE',  ( -1.000000000000000000, 0.000000000000000000, 0.000000000000000000 ) ) ;
#6452 = CARTESIAN_POINT ( 'NONE',  ( -2.472591809326046608, 28.89829686842208289, 13.04906658473306891 ) ) ;
#6453 = DIRECTION ( 'NONE',  ( 0.000000000000000000, 0.000000000000000000, 1.000000000000000000 ) ) ;
#6454 = CONICAL_SURFACE ( 'NONE', #6115, 1.649999999999998579, 1.029744258676653423 ) ;
#6455 = ORIENTED_EDGE ( 'NONE', *, *, #8988, .F. ) ;
#6456 = CARTESIAN_POINT ( 'NONE',  ( 2.887392608830354757, -4.041451884327390331, 2.328390191177121598E-14 ) ) ;
#6457 = ORIENTED_EDGE ( 'NONE', *, *, #5607, .F. ) ;
#6458 = CARTESIAN_POINT ( 'NONE',  ( 2.527408190673967159, 30.96936468028756906, 15.66968341526694175 ) ) ;
#6459 = COLOUR_RGB ( '', 0.31764706, 0.68627451, 0.89019608) ;
#6460 = CARTESIAN_POINT ( 'NONE',  ( -4.000000000000000000, 0.8576368993457507139, -3.433240632782198709 ) ) ;
#6461 = VECTOR ( 'NONE', #6851, 1000.000000000000000 ) ;
#6462 =( BOUNDED_CURVE ( )  B_SPLINE_CURVE ( 1, ( #8279, #550 ),
 .UNSPECIFIED., .F., .F. ) 
 B_SPLINE_CURVE_WITH_KNOTS ( ( 2, 2 ),
 ( 0.000000000000000000, 1.000000000000000000 ),
 .UNSPECIFIED. ) 
 CURVE ( )  GEOMETRIC_REPRESENTATION_ITEM ( )  RATIONAL_B_SPLINE_CURVE ( ( 0.9343183816103359796, 0.9343183816103359796 ) ) 
 REPRESENTATION_ITEM ( '' )  );
#6463 = CARTESIAN_POINT ( 'NONE',  ( 29.49999999999999645, 1.387778780781445676E-14, -12.49999999999999822 ) ) ;
#6464 = CONICAL_SURFACE ( 'NONE', #10959, 1664.279482350528269, 1.029744258676657198 ) ;
#6465 = CARTESIAN_POINT ( 'NONE',  ( 4.000000000000000000, -2.309401076758514915, -3.433295621305383349 ) ) ;
#6466 = EDGE_CURVE ( 'NONE', #2261, #6168, #4291, .T. ) ;
#6467 = PLANE ( 'NONE',  #9144 ) ;
#6468 = CARTESIAN_POINT ( 'NONE',  ( -26.79131905728310059, 50.65208333237728766, -6.403925809002825709 ) ) ;
#6469 = EDGE_CURVE ( 'NONE', #5040, #1717, #144, .T. ) ;
#6470 = CARTESIAN_POINT ( 'NONE',  ( 6.015568632492056977, 34.47916666666665009, -2.499999999999998668 ) ) ;
#6471 = CARTESIAN_POINT ( 'NONE',  ( -1.390230914382372118, -4.043987460488664532, -3.502507215260523665 ) ) ;
#6472 = EDGE_LOOP ( 'NONE', ( #5031, #6059, #3543, #596 ) ) ;
#6473 = VECTOR ( 'NONE', #2746, 1000.000000000000000 ) ;
#6474 = CARTESIAN_POINT ( 'NONE',  ( -25.98076211353310683, 54.13749999808803182, -3.000000000000132339 ) ) ;
#6475 = CIRCLE ( 'NONE', #7913, 1.649999999999989919 ) ;
#6476 = LINE ( 'NONE', #8044, #5923 ) ;
#6477 = CARTESIAN_POINT ( 'NONE',  ( -26.98076211353408382, 57.99999999999985789, -9.000000000000701661 ) ) ;
#6478 = ADVANCED_FACE ( 'NONE', ( #7796 ), #3152, .F. ) ;
#6479 = CARTESIAN_POINT ( 'NONE',  ( -27.60187600103308725, 54.91041666571061342, -5.935950539335252074 ) ) ;
#6480 = CARTESIAN_POINT ( 'NONE',  ( 22.10027471249113162, 22.50626116107413921, 11.00732503135576401 ) ) ;
#6481 = CARTESIAN_POINT ( 'NONE',  ( -24.35964822603314772, 53.86041666571062336, -4.064049460664953983 ) ) ;
#6482 = EDGE_LOOP ( 'NONE', ( #1212, #799, #6445, #10995 ) ) ;
#6483 = EDGE_CURVE ( 'NONE', #6485, #170, #4762, .T. ) ;
#6484 = CARTESIAN_POINT ( 'NONE',  ( 34.93845944406324122, 2.080102445711406123, 4.707808283735069210 ) ) ;
#6485 = VERTEX_POINT ( 'NONE', #3567 ) ;
#6486 = VERTEX_POINT ( 'NONE', #10339 ) ;
#6487 = DIRECTION ( 'NONE',  ( 0.000000000000000000, 0.4999999999999993339, -0.8660254037844390407 ) ) ;
#6488 = ORIENTED_EDGE ( 'NONE', *, *, #3774, .F. ) ;
#6489 = DIRECTION ( 'NONE',  ( -1.000000000000000000, -0.000000000000000000, -0.000000000000000000 ) ) ;
#6490 = AXIS2_PLACEMENT_3D ( 'NONE', #8469, #4255, #14 ) ;
#6491 = ORIENTED_EDGE ( 'NONE', *, *, #7162, .T. ) ;
#6492 = CARTESIAN_POINT ( 'NONE',  ( 15.36174878203077476, 18.17378512388119915, 11.22291988893967840 ) ) ;
#6493 =( NAMED_UNIT ( * ) PLANE_ANGLE_UNIT ( ) SI_UNIT ( $, .RADIAN. ) );
#6494 = EDGE_CURVE ( 'NONE', #2929, #647, #1618, .T. ) ;
#6495 = CARTESIAN_POINT ( 'NONE',  ( 16.90694777372845437, 16.62861179130368683, 12.08020438729360180 ) ) ;
#6496 = CARTESIAN_POINT ( 'NONE',  ( -24.98076211353313170, 53.49583333142136610, -3.267949192431250705 ) ) ;
#6497 = CARTESIAN_POINT ( 'NONE',  ( 0.000000000000000000, 30.00000000000000000, 2.500000000000000000 ) ) ;
#6498 = CYLINDRICAL_SURFACE ( 'NONE', #2988, 2.149999999999992362 ) ;
#6499 = ORIENTED_EDGE ( 'NONE', *, *, #9675, .F. ) ;
#6500 = PRODUCT_DEFINITION_FORMATION_WITH_SPECIFIED_SOURCE ( 'ANY', '', #7680, .NOT_KNOWN. ) ;
#6501 = ORIENTED_EDGE ( 'NONE', *, *, #10765, .T. ) ;
#6502 = CARTESIAN_POINT ( 'NONE',  ( 16.78877909162549642, 18.16096837667994279, 13.15979613361243494 ) ) ;
#6503 = CARTESIAN_POINT ( 'NONE',  ( -25.98076211353311393, 52.47499999999985931, -7.000000000000072831 ) ) ;
#6504 = CIRCLE ( 'NONE', #656, 4.000000000000600409 ) ;
#6505 = AXIS2_PLACEMENT_3D ( 'NONE', #6192, #7087, #5419 ) ;
#6506 = FACE_OUTER_BOUND ( 'NONE', #2353, .T. ) ;
#6507 = CARTESIAN_POINT ( 'NONE',  ( 29.49999999999999645, -3.999999999999983569, 10.00000000000000888 ) ) ;
#6508 = CARTESIAN_POINT ( 'NONE',  ( -2.527408190673963162, 30.96936468028755840, 14.14281658473306713 ) ) ;
#6509 = DIRECTION ( 'NONE',  ( 1.000000000000000000, 0.000000000000000000, 0.000000000000000000 ) ) ;
#6510 = ORIENTED_EDGE ( 'NONE', *, *, #10590, .F. ) ;
#6511 = CARTESIAN_POINT ( 'NONE',  ( -25.98076211353311393, 51.33749999808802755, -3.000000000000132783 ) ) ;
#6512 = VERTEX_POINT ( 'NONE', #2566 ) ;
#6513 = CONICAL_SURFACE ( 'NONE', #10781, 2.041999999999999815, 1.047197551196591858 ) ;
#6514 = CARTESIAN_POINT ( 'NONE',  ( 1.101703131577913553, 32.47259180932605460, 14.57593341526694175 ) ) ;
#6515 = CARTESIAN_POINT ( 'NONE',  ( -25.98076211353311038, 61.49999999999985789, -1.499999999999510392 ) ) ;
#6516 = EDGE_CURVE ( 'NONE', #3385, #7860, #1733, .T. ) ;
#6517 = CARTESIAN_POINT ( 'NONE',  ( -23.98076211353314235, 52.27083333142136468, -6.154700538379337615 ) ) ;
#6518 = CARTESIAN_POINT ( 'NONE',  ( 0.000000000000000000, 0.000000000000000000, 0.000000000000000000 ) ) ;
#6519 = CARTESIAN_POINT ( 'NONE',  ( 34.99999999999987210, -3.999999999999989786, 9.999999999999998224 ) ) ;
#6520 = CARTESIAN_POINT ( 'NONE',  ( -24.35964822603314772, 51.87708333237728908, -5.935950539335252074 ) ) ;
#6521 = FACE_OUTER_BOUND ( 'NONE', #6954, .T. ) ;
#6522 = CIRCLE ( 'NONE', #3003, 4.999999999999997335 ) ;
#6523 = COLOUR_RGB ( '', 0.31764706, 0.68627451, 0.89019608) ;
#6524 = CARTESIAN_POINT ( 'NONE',  ( 0.000000000000000000, 0.000000000000000000, 3.249999999999998224 ) ) ;
#6525 = ORIENTED_EDGE ( 'NONE', *, *, #253, .F. ) ;
#6526 = AXIS2_PLACEMENT_3D ( 'NONE', #9301, #79, #3483 ) ;
#6527 = CARTESIAN_POINT ( 'NONE',  ( 3.500000000000007550, 28.55025253169416644, 14.51562500000000355 ) ) ;
#6528 = PRODUCT_DEFINITION ( 'UNKNOWN', '', #6500, #10891 ) ;
#6529 = DIRECTION ( 'NONE',  ( 0.000000000000000000, 1.000000000000000000, 0.000000000000000000 ) ) ;
#6530 = EDGE_CURVE ( 'NONE', #6697, #9804, #5015, .T. ) ;
#6531 =( BOUNDED_CURVE ( )  B_SPLINE_CURVE ( 2, ( #9553, #1099, #5122, #10224, #8500, #4505, #5173, #4337, #880 ),
 .UNSPECIFIED., .F., .F. ) 
 B_SPLINE_CURVE_WITH_KNOTS ( ( 3, 2, 2, 2, 3 ),
 ( 0.2500000000000000000, 0.2592592592592592449, 0.2777777777777777901, 0.2962962962962962798, 0.3055555555555555802 ),
 .UNSPECIFIED. ) 
 CURVE ( )  GEOMETRIC_REPRESENTATION_ITEM ( )  RATIONAL_B_SPLINE_CURVE ( ( 0.9330127018922192983, 0.9330127018922194093, 1.000000000000000000, 0.8660254037844387076, 1.000000000000000000, 0.8660254037844387076, 1.000000000000000000, 0.9330127018922191873, 0.9330127018922194093 ) ) 
 REPRESENTATION_ITEM ( '' )  );
#6532 = EDGE_CURVE ( 'NONE', #5764, #10879, #6828, .T. ) ;
#6533 = FACE_OUTER_BOUND ( 'NONE', #1577, .T. ) ;
#6534 = B_SPLINE_CURVE_WITH_KNOTS ( 'NONE', 3,
 ( #9691, #5475, #8909, #1925, #4640, #10583, #3693, #5312, #1073, #10417 ),
 .UNSPECIFIED., .F., .F.,
 ( 4, 2, 2, 2, 4 ),
 ( 0.003180982857628660964, 0.003578183968417414373, 0.003975385079206167349, 0.004372586189994920325, 0.004769787300783674168 ),
 .UNSPECIFIED. ) ;
#6535 = CARTESIAN_POINT ( 'NONE',  ( -25.98076211353310683, 53.04374999904395338, -3.128098921329806714 ) ) ;
#6536 = CARTESIAN_POINT ( 'NONE',  ( 19.89794927727885110, 21.35687623891577758, 11.00732503135556861 ) ) ;
#6537 = CARTESIAN_POINT ( 'NONE',  ( -23.98076211353314235, 50.14166666666653072, -3.845299461620867554 ) ) ;
#6538 = ORIENTED_EDGE ( 'NONE', *, *, #4506, .T. ) ;
#6539 = CARTESIAN_POINT ( 'NONE',  ( -27.60187600103308370, 55.84374999904394343, -5.000000000000103029 ) ) ;
#6540 = EDGE_CURVE ( 'NONE', #8562, #3014, #1387, .T. ) ;
#6541 = ORIENTED_EDGE ( 'NONE', *, *, #9942, .T. ) ;
#6542 = VERTEX_POINT ( 'NONE', #10233 ) ;
#6543 = DIRECTION ( 'NONE',  ( 0.9876851083892502770, 0.1564548710207356030, 0.000000000000000000 ) ) ;
#6545 = VERTEX_POINT ( 'NONE', #7065 ) ;
#6544 = EDGE_CURVE ( 'NONE', #4598, #7957, #3513, .T. ) ;
#6546 = CARTESIAN_POINT ( 'NONE',  ( -21.21106610644865498, 13.49999999999941913, -5.000000000000000000 ) ) ;
#6547 =( NAMED_UNIT ( * ) PLANE_ANGLE_UNIT ( ) SI_UNIT ( $, .RADIAN. ) );
#6548 = EDGE_LOOP ( 'NONE', ( #5842, #6886, #10522, #6207 ) ) ;
#6549 = CARTESIAN_POINT ( 'NONE',  ( 19.91130943667480224, 20.32997460694367575, 11.00732503135576401 ) ) ;
#6550 = FACE_OUTER_BOUND ( 'NONE', #650, .T. ) ;
#6551 = FACE_OUTER_BOUND ( 'NONE', #10396, .T. ) ;
#6552 = CARTESIAN_POINT ( 'NONE',  ( 19.39692024064573062, 16.06847318657456469, 12.95562166920678138 ) ) ;
#6553 = CARTESIAN_POINT ( 'NONE',  ( -27.98076211353308551, 50.46249999808803466, -5.000000000000103029 ) ) ;
#6554 = CARTESIAN_POINT ( 'NONE',  ( 34.85635190221861279, 3.172051726186626563, -3.113055717248543797 ) ) ;
#6555 = CARTESIAN_POINT ( 'NONE',  ( 0.000000000000000000, 0.000000000000000000, -2.000000000000000000 ) ) ;
#6556 = ORIENTED_EDGE ( 'NONE', *, *, #3762, .T. ) ;
#6557 = CARTESIAN_POINT ( 'NONE',  ( -1.734723475976807094E-15, 33.50000000000000000, 13.65625000000000355 ) ) ;
#6558 = ORIENTED_EDGE ( 'NONE', *, *, #457, .T. ) ;
#6559 = CARTESIAN_POINT ( 'NONE',  ( 21.93767140838681584, 18.93041396519599928, 13.00425721518307576 ) ) ;
#6560 = LINE ( 'NONE', #9850, #2053 ) ;
#6561 = CARTESIAN_POINT ( 'NONE',  ( 1.047444401652940007E-13, 30.00000000000000000, -2.500000000000000000 ) ) ;
#6562 = CARTESIAN_POINT ( 'NONE',  ( -1.655952806101422814, 3.662737355149034979, -7.623296525288699970E-18 ) ) ;
#6563 = CARTESIAN_POINT ( 'NONE',  ( -0.9693646802875608426, 27.47259180932603684, 14.45531658473306535 ) ) ;
#6564 = DIRECTION ( 'NONE',  ( 1.000000000000000000, 0.000000000000000000, 0.000000000000000000 ) ) ;
#6565 = ORIENTED_EDGE ( 'NONE', *, *, #8934, .T. ) ;
#6566 = DIRECTION ( 'NONE',  ( 0.000000000000000000, 1.000000000000000000, 0.000000000000000000 ) ) ;
#6567 = EDGE_LOOP ( 'NONE', ( #2107, #7052, #3889, #10166, #10507 ) ) ;
#6568 = CARTESIAN_POINT ( 'NONE',  ( -2.500000000000007550, 30.06616922564517580, 17.46655841526694175 ) ) ;
#6569 = CARTESIAN_POINT ( 'NONE',  ( 34.99999999999999289, -9.999999999999998224, -12.49999999999999822 ) ) ;
#6570 = FACE_OUTER_BOUND ( 'NONE', #7638, .T. ) ;
#6571 = DIRECTION ( 'NONE',  ( -0.5150380749100518241, 0.000000000000000000, 0.8571673007021137769 ) ) ;
#6572 = CARTESIAN_POINT ( 'NONE',  ( 4.000000000000000000, 2.309401076758497151, -3.433295621305379353 ) ) ;
#6573 = CARTESIAN_POINT ( 'NONE',  ( -25.98076211353311393, 50.59374999904395054, -6.871901078670400231 ) ) ;
#6574 = CARTESIAN_POINT ( 'NONE',  ( 0.3461262719736147297, -4.658553426539303821, -3.671615880910379381 ) ) ;
#6575 = DIRECTION ( 'NONE',  ( 0.000000000000000000, 0.000000000000000000, -1.000000000000000000 ) ) ;
#6576 = ORIENTED_EDGE ( 'NONE', *, *, #8859, .F. ) ;
#6577 = CARTESIAN_POINT ( 'NONE',  ( -3.500000000000003997, 31.44974746830583001, 15.14062500000000355 ) ) ;
#6578 = DIRECTION ( 'NONE',  ( 1.000000000000000000, 0.000000000000000000, 0.000000000000000000 ) ) ;
#6579 = CARTESIAN_POINT ( 'NONE',  ( -26.79131905728310059, 50.82708333237727771, -6.403925809002825709 ) ) ;
#6580 = CARTESIAN_POINT ( 'NONE',  ( -26.79131905728310059, 52.05208333237728624, -6.403925809002825709 ) ) ;
#6581 = CARTESIAN_POINT ( 'NONE',  ( 22.42490604353609029, 22.35994869845890065, 11.00732503135576401 ) ) ;
#6582 = CARTESIAN_POINT ( 'NONE',  ( -23.98076211353314235, 51.59999999999985931, -5.000000000000103029 ) ) ;
#6583 = AXIS2_PLACEMENT_3D ( 'NONE', #5925, #6091, #9313 ) ;
#6584 = EDGE_LOOP ( 'NONE', ( #10785, #7734, #7115, #8634 ) ) ;
#6585 = CARTESIAN_POINT ( 'NONE',  ( 34.82458596820516306, 3.503579405888650466, 2.892497030208068143 ) ) ;
#6586 = ORIENTED_EDGE ( 'NONE', *, *, #7144, .F. ) ;
#6587 = ORIENTED_EDGE ( 'NONE', *, *, #6615, .T. ) ;
#6588 = CARTESIAN_POINT ( 'NONE',  ( -0.6920835326022555245, -4.454600218803899558, -3.597382984111586079 ) ) ;
#6589 = ORIENTED_EDGE ( 'NONE', *, *, #603, .F. ) ;
#6590 = CARTESIAN_POINT ( 'NONE',  ( 25.58039891549807976, 2.000000000000001776, -2.500000000000000444 ) ) ;
#6591 = CARTESIAN_POINT ( 'NONE',  ( 0.000000000000000000, 0.000000000000000000, 0.000000000000000000 ) ) ;
#6592 = EDGE_LOOP ( 'NONE', ( #4999, #7392 ) ) ;
#6593 = CARTESIAN_POINT ( 'NONE',  ( 23.28338686706186778, 20.94194386221399640, 11.00732503135556861 ) ) ;
#6594 = CIRCLE ( 'NONE', #3063, 2.149999999999994582 ) ;
#6595 = CARTESIAN_POINT ( 'NONE',  ( 25.98076211353311749, 56.49999999999984368, 12.14999999999999503 ) ) ;
#6596 = EDGE_CURVE ( 'NONE', #1634, #8162, #277, .T. ) ;
#6597 = CARTESIAN_POINT ( 'NONE',  ( -4.101948962585905356, -2.368261337751088824, -3.681124513963624167 ) ) ;
#6598 = EDGE_CURVE ( 'NONE', #6989, #8234, #2122, .T. ) ;
#6599 = CARTESIAN_POINT ( 'NONE',  ( 24.14247934234231963, 22.08663129433533001, 12.94889058896630019 ) ) ;
#6600 = CARTESIAN_POINT ( 'NONE',  ( -27.98076211353308551, 52.62083333142137320, -3.845299461620869330 ) ) ;
#6601 = CARTESIAN_POINT ( 'NONE',  ( -25.98076211353311393, 53.17499999999985505, -7.000000000000072831 ) ) ;
#6602 = CARTESIAN_POINT ( 'NONE',  ( -31.74999999999995737, 5.204748896376250699E-16, -4.250000000000000000 ) ) ;
#6603 = EDGE_LOOP ( 'NONE', ( #4215, #7834, #9094, #10352 ) ) ;
#6604 = CARTESIAN_POINT ( 'NONE',  ( -3.472591809326048384, 31.51591669395100936, 16.13843341526694530 ) ) ;
#6605 = ORIENTED_EDGE ( 'NONE', *, *, #6038, .F. ) ;
#6606 = CARTESIAN_POINT ( 'NONE',  ( 16.95349311633468403, 16.58206632678699677, 13.07803561935715742 ) ) ;
#6607 = EDGE_CURVE ( 'NONE', #8989, #7545, #7407, .T. ) ;
#6608 = CARTESIAN_POINT ( 'NONE',  ( -25.98076211353311393, 52.12499999999985079, -3.000000000000132339 ) ) ;
#6609 = LINE ( 'NONE', #8397, #9600 ) ;
#6610 = CARTESIAN_POINT ( 'NONE',  ( -26.95376948895698987, 57.73464630110304796, -3.251713298125628704 ) ) ;
#6611 = CARTESIAN_POINT ( 'NONE',  ( -0.9693646802875608426, 27.47259180932603684, 13.20531658473306713 ) ) ;
#6612 = CARTESIAN_POINT ( 'NONE',  ( 16.58601566935801586, 18.36373179894819074, 12.17661548709639696 ) ) ;
#6613 = EDGE_LOOP ( 'NONE', ( #4525, #2461, #8996, #10753, #9685 ) ) ;
#6614 = CARTESIAN_POINT ( 'NONE',  ( -26.51666049839535688, 55.21876073720499534, -7.000000000000071942 ) ) ;
#6615 = EDGE_CURVE ( 'NONE', #1334, #2779, #2062, .T. ) ;
#6616 = ORIENTED_EDGE ( 'NONE', *, *, #7769, .F. ) ;
#6617 = AXIS2_PLACEMENT_3D ( 'NONE', #6005, #1670, #1789 ) ;
#6618 = ORIENTED_EDGE ( 'NONE', *, *, #8406, .F. ) ;
#6619 = DIRECTION ( 'NONE',  ( -1.000000000000000000, -0.000000000000000000, -0.000000000000000000 ) ) ;
#6620 = CARTESIAN_POINT ( 'NONE',  ( -25.98076211353311393, 54.83749999808802755, -3.000000000000132339 ) ) ;
#6621 = DIRECTION ( 'NONE',  ( -0.000000000000000000, -0.000000000000000000, -1.000000000000000000 ) ) ;
#6622 = DIRECTION ( 'NONE',  ( -1.000000000000000000, -0.000000000000000000, -0.000000000000000000 ) ) ;
#6623 = DIRECTION ( 'NONE',  ( -0.000000000000000000, -0.000000000000000000, -1.000000000000000000 ) ) ;
#6624 = CARTESIAN_POINT ( 'NONE',  ( -25.17020516978313083, 49.83541666571061768, -6.403925809002825709 ) ) ;
#6625 = AXIS2_PLACEMENT_3D ( 'NONE', #6036, #1705, #10923 ) ;
#6626 = EDGE_CURVE ( 'NONE', #4583, #3723, #2639, .T. ) ;
#6627 = CARTESIAN_POINT ( 'NONE',  ( 2.000000000000000000, -0.8865213383406694847, 1.535500000000001419 ) ) ;
#6628 = DIRECTION ( 'NONE',  ( 0.000000000000000000, -1.000000000000000000, 0.000000000000000000 ) ) ;
#6629 = ORIENTED_EDGE ( 'NONE', *, *, #905, .F. ) ;
#6630 = CARTESIAN_POINT ( 'NONE',  ( 2.474873734152918558, 32.47487373415292211, 13.50000000000000355 ) ) ;
#6631 = AXIS2_PLACEMENT_3D ( 'NONE', #2829, #4653, #6371 ) ;
#6632 = CARTESIAN_POINT ( 'NONE',  ( -30.75045812061784289, 13.49999999999941913, -9.500000000000000000 ) ) ;
#6633 = CARTESIAN_POINT ( 'NONE',  ( 24.55500000000002103, 0.000000000000000000, 2.500000000000001332 ) ) ;
#6634 = VECTOR ( 'NONE', #7832, 999.9999999999998863 ) ;
#6635 = DIRECTION ( 'NONE',  ( -0.000000000000000000, -1.000000000000000000, -0.000000000000000000 ) ) ;
#6636 = EDGE_CURVE ( 'NONE', #4849, #6073, #6271, .T. ) ;
#6637 = CARTESIAN_POINT ( 'NONE',  ( -25.98076211353310683, 51.64374999904395480, -3.128098921329806714 ) ) ;
#6638 =( GEOMETRIC_REPRESENTATION_CONTEXT ( 3 ) GLOBAL_UNCERTAINTY_ASSIGNED_CONTEXT ( ( #7586 ) ) GLOBAL_UNIT_ASSIGNED_CONTEXT ( ( #8442, #4958, #6657 ) ) REPRESENTATION_CONTEXT ( 'NONE', 'WORKASPACE' ) );
#6639 = AXIS2_PLACEMENT_3D ( 'NONE', #1685, #3471, #10299 ) ;
#6640 = CARTESIAN_POINT ( 'NONE',  ( 20.43380676890320657, 22.25420293214091316, 12.00579112326941988 ) ) ;
#6641 = CARTESIAN_POINT ( 'NONE',  ( -23.98076211353314235, 52.35833333333319928, -6.154700538379337615 ) ) ;
#6642 = VECTOR ( 'NONE', #10648, 1000.000000000000000 ) ;
#6643 = AXIS2_PLACEMENT_3D ( 'NONE', #6215, #7057, #7265 ) ;
#6644 = VERTEX_POINT ( 'NONE', #2851 ) ;
#6645 = ORIENTED_EDGE ( 'NONE', *, *, #2417, .F. ) ;
#6646 = ORIENTED_EDGE ( 'NONE', *, *, #10826, .T. ) ;
#6647 = CARTESIAN_POINT ( 'NONE',  ( -25.98076211353324894, 4.999999999999997335, 5.500000000000000000 ) ) ;
#6648 = ORIENTED_EDGE ( 'NONE', *, *, #9460, .F. ) ;
#6649 = CARTESIAN_POINT ( 'NONE',  ( 2.500000000000007550, 31.03553390593274486, 15.92187500000000178 ) ) ;
#6650 = DIRECTION ( 'NONE',  ( 1.000000000000000000, 0.000000000000000000, 0.000000000000000000 ) ) ;
#6651 = AXIS2_PLACEMENT_3D ( 'NONE', #7357, #4084, #3190 ) ;
#6652 = ORIENTED_EDGE ( 'NONE', *, *, #7454, .T. ) ;
#6653 = CARTESIAN_POINT ( 'NONE',  ( 20.46928886811658188, 22.21026755401432240, 11.00732503135576401 ) ) ;
#6654 = FILL_AREA_STYLE ('',( #10881 ) ) ;
#6655 = VECTOR ( 'NONE', #4821, 1000.000000000000114 ) ;
#6656 = EDGE_CURVE ( 'NONE', #2434, #1386, #5342, .T. ) ;
#6657 =( NAMED_UNIT ( * ) SI_UNIT ( $, .STERADIAN. ) SOLID_ANGLE_UNIT ( ) );
#6658 = CARTESIAN_POINT ( 'NONE',  ( -24.35964822603314772, 50.65208333237728056, -5.935950539335252074 ) ) ;
#6659 = CARTESIAN_POINT ( 'NONE',  ( 18.83541841558448837, 19.97999999654625825, 12.94889058896590583 ) ) ;
#6660 = CARTESIAN_POINT ( 'NONE',  ( 0.000000000000000000, 0.000000000000000000, 0.000000000000000000 ) ) ;
#6661 = CARTESIAN_POINT ( 'NONE',  ( -25.98076211353311393, 55.18749999808802897, -7.309401076758571314 ) ) ;
#6662 = VECTOR ( 'NONE', #3634, 1000.000000000000000 ) ;
#6663 = CARTESIAN_POINT ( 'NONE',  ( -4.198928548860774157, 0.8158838809860065044, -3.526471437616918170 ) ) ;
#6664 = ORIENTED_EDGE ( 'NONE', *, *, #1654, .T. ) ;
#6665 = FACE_OUTER_BOUND ( 'NONE', #4555, .T. ) ;
#6666 = PRODUCT_DEFINITION_CONTEXT ( 'detailed design', #10409, 'design' ) ;
#6667 = ORIENTED_EDGE ( 'NONE', *, *, #8499, .F. ) ;
#6668 = CARTESIAN_POINT ( 'NONE',  ( -3.472591809326048384, 31.51591669395100936, 17.38843341526693820 ) ) ;
#6669 = ORIENTED_EDGE ( 'NONE', *, *, #5734, .F. ) ;
#6670 = EDGE_CURVE ( 'NONE', #7102, #7683, #2793, .T. ) ;
#6671 = CARTESIAN_POINT ( 'NONE',  ( 21.33873319047917150, 17.29751440752404434, 12.94889058896590583 ) ) ;
#6672 = EDGE_CURVE ( 'NONE', #2549, #10302, #4464, .T. ) ;
#6673 = B_SPLINE_CURVE_WITH_KNOTS ( 'NONE', 3,
 ( #10834, #3116, #442, #10672, #601, #3896 ),
 .UNSPECIFIED., .F., .F.,
 ( 4, 2, 4 ),
 ( 0.003657268138676097926, 0.004679653797516874353, 0.005702039456357650346 ),
 .UNSPECIFIED. ) ;
#6674 = AXIS2_PLACEMENT_3D ( 'NONE', #5869, #10262, #9307 ) ;
#6675 = CARTESIAN_POINT ( 'NONE',  ( -25.36399665479294896, 58.79766018380388459, -6.905020239873124410 ) ) ;
#6676 = DIRECTION ( 'NONE',  ( 0.000000000000000000, 0.000000000000000000, 1.000000000000000000 ) ) ;
#6677 = CARTESIAN_POINT ( 'NONE',  ( -26.98076211353408027, 57.86781137917856910, -3.267949192431818251 ) ) ;
#6678 = CARTESIAN_POINT ( 'NONE',  ( -1.383578242660655100, 26.47259180932604039, 13.20531658473306713 ) ) ;
#6679 = CARTESIAN_POINT ( 'NONE',  ( 34.99999999999987210, -3.999999999999989786, 12.14999999999999503 ) ) ;
#6680 = PLANE ( 'NONE',  #8243 ) ;
#6681 = CARTESIAN_POINT ( 'NONE',  ( 3.199999999999999734, 0.000000000000000000, 3.499999999999999556 ) ) ;
#6682 = ORIENTED_EDGE ( 'NONE', *, *, #9409, .T. ) ;
#6683 = ADVANCED_FACE ( 'NONE', ( #6330 ), #8728, .T. ) ;
#6684 = ORIENTED_EDGE ( 'NONE', *, *, #8120, .T. ) ;
#6685 = CARTESIAN_POINT ( 'NONE',  ( -25.98076211353311393, 51.77499999999986358, -7.000000000000072831 ) ) ;
#6686 = CARTESIAN_POINT ( 'NONE',  ( -3.999999999998910649, -1.658469974638591804, -3.531532913075256186 ) ) ;
#6687 =( GEOMETRIC_REPRESENTATION_CONTEXT ( 3 ) GLOBAL_UNCERTAINTY_ASSIGNED_CONTEXT ( ( #6199 ) ) GLOBAL_UNIT_ASSIGNED_CONTEXT ( ( #3838, #3013, #5619 ) ) REPRESENTATION_CONTEXT ( 'NONE', 'WORKASPACE' ) );
#6688 = CARTESIAN_POINT ( 'NONE',  ( 34.69578914996071717, 4.608685395970378629, -2.519144107514305730 ) ) ;
#6689 = CARTESIAN_POINT ( 'NONE',  ( 34.99999999999999289, -3.999999999999993339, 7.850000000000012967 ) ) ;
#6690 = ADVANCED_FACE ( 'NONE', ( #7953 ), #7846, .T. ) ;
#6691 = EDGE_CURVE ( 'NONE', #8565, #947, #1894, .T. ) ;
#6692 = DIRECTION ( 'NONE',  ( -1.000000000000000000, 0.000000000000000000, 0.000000000000000000 ) ) ;
#6693 = CARTESIAN_POINT ( 'NONE',  ( -24.35964822603314772, 55.43541666571061199, -4.064049460664953983 ) ) ;
#6694 = B_SPLINE_CURVE_WITH_KNOTS ( 'NONE', 3,
 ( #10766, #10664, #5667, #6386, #3106, #10821, #6585, #3008, #6430, #5765, #7217, #9829, #2275, #6484, #7321, #1389 ),
 .UNSPECIFIED., .F., .F.,
 ( 4, 2, 2, 2, 2, 2, 2, 4 ),
 ( 0.000000000000000000, 0.0005875779155018993763, 0.001175155831003798753, 0.001762733746505697804, 0.002350311662007597505, 0.002937889577509496773, 0.003525467493011394740, 0.004700623324015191541 ),
 .UNSPECIFIED. ) ;
#6695 = LINE ( 'NONE', #1813, #1398 ) ;
#6696 = CARTESIAN_POINT ( 'NONE',  ( 5.000000000000000888, 0.000000000000000000, 0.000000000000000000 ) ) ;
#6697 = VERTEX_POINT ( 'NONE', #5394 ) ;
#6698 = AXIS2_PLACEMENT_3D ( 'NONE', #7004, #3616, #9504 ) ;
#6699 = CIRCLE ( 'NONE', #8659, 4.999999999999997335 ) ;
#6700 = CARTESIAN_POINT ( 'NONE',  ( -2.000000000000006661, 3.464101615137750834, 0.000000000000000000 ) ) ;
#6701 = CARTESIAN_POINT ( 'NONE',  ( -27.60187600103308370, 53.74374999904394201, -5.000000000000103029 ) ) ;
#6702 = CARTESIAN_POINT ( 'NONE',  ( -25.98076211353310683, 52.69374999904395196, -6.871901078670399343 ) ) ;
#6703 = VECTOR ( 'NONE', #6709, 1000.000000000000000 ) ;
#6704 = STYLED_ITEM ( 'NONE', ( #598 ), #7322 ) ;
#6705 = AXIS2_PLACEMENT_3D ( 'NONE', #1643, #6802, #5038 ) ;
#6706 = DIRECTION ( 'NONE',  ( 1.000000000000000000, -0.000000000000000000, -0.000000000000000000 ) ) ;
#6707 = CARTESIAN_POINT ( 'NONE',  ( -24.98076211353312814, 53.11666666666652503, -6.732050807568954909 ) ) ;
#6708 = ORIENTED_EDGE ( 'NONE', *, *, #10435, .T. ) ;
#6709 = DIRECTION ( 'NONE',  ( -0.000000000000000000, -0.000000000000000000, 1.000000000000000000 ) ) ;
#6710 = EDGE_CURVE ( 'NONE', #3494, #3024, #217, .T. ) ;
#6711 = ORIENTED_EDGE ( 'NONE', *, *, #8671, .F. ) ;
#6712 = ORIENTED_EDGE ( 'NONE', *, *, #3077, .T. ) ;
#6713 = CARTESIAN_POINT ( 'NONE',  ( 34.94281041931228771, 2.000000000000002220, -5.500000000000000000 ) ) ;
#6714 = ORIENTED_EDGE ( 'NONE', *, *, #2398, .F. ) ;
#6715 = MECHANICAL_DESIGN_GEOMETRIC_PRESENTATION_REPRESENTATION (  '', ( #5307 ), #307 ) ;
#6716 = DIRECTION ( 'NONE',  ( -0.000000000000000000, -0.000000000000000000, -1.000000000000000000 ) ) ;
#6717 = ORIENTED_EDGE ( 'NONE', *, *, #3563, .F. ) ;
#6718 = CIRCLE ( 'NONE', #4057, 1.649999999999998579 ) ;
#6719 = CARTESIAN_POINT ( 'NONE',  ( 22.84119893477061680, 19.75612935582806529, 11.00732503135576401 ) ) ;
#6720 = CARTESIAN_POINT ( 'NONE',  ( 0.2500000000000002220, 0.000000000000000000, 0.000000000000000000 ) ) ;
#6721 = CARTESIAN_POINT ( 'NONE',  ( 29.50000000000000711, -9.999999999999998224, 15.49999999999998934 ) ) ;
#6722 = CARTESIAN_POINT ( 'NONE',  ( 17.31044041986821469, 16.31370680995936695, 13.04945978079559765 ) ) ;
#6723 = CYLINDRICAL_SURFACE ( 'NONE', #8141, 34.99999999999999289 ) ;
#6724 = CARTESIAN_POINT ( 'NONE',  ( -24.98076211353312814, 54.42916666475469611, -6.732050807568954909 ) ) ;
#6725 = CARTESIAN_POINT ( 'NONE',  ( -4.211140560182196957, 2.431303136016537803, -3.745885042887433514 ) ) ;
#6726 = VERTEX_POINT ( 'NONE', #7219 ) ;
#6727 = CARTESIAN_POINT ( 'NONE',  ( -26.98076211353309972, 50.34583333142136752, -6.732050807568954909 ) ) ;
#6728 = ORIENTED_EDGE ( 'NONE', *, *, #5228, .F. ) ;
#6729 = CARTESIAN_POINT ( 'NONE',  ( -3.527408190673960053, 31.38357824266065066, 12.89281658473306535 ) ) ;
#6730 = EDGE_LOOP ( 'NONE', ( #5937, #9639, #1040, #9613 ) ) ;
#6731 = CARTESIAN_POINT ( 'NONE',  ( 19.39692024064573062, 16.06847318657456469, 12.95562166920678138 ) ) ;
#6732 = LINE ( 'NONE', #2575, #444 ) ;
#6733 = LINE ( 'NONE', #7400, #5310 ) ;
#6734 = CARTESIAN_POINT ( 'NONE',  ( -26.24738432486657302, 57.02739972993323647, -3.014058635233636707 ) ) ;
#6735 = CARTESIAN_POINT ( 'NONE',  ( 4.553649124439118623E-15, 27.49999999999999289, 14.28125000000000355 ) ) ;
#6736 = CARTESIAN_POINT ( 'NONE',  ( -24.98076211353312814, 51.62916666475469896, -6.732050807568954909 ) ) ;
#6737 = CARTESIAN_POINT ( 'NONE',  ( 29.49999999999999645, -3.999999999999983569, 10.00000000000000888 ) ) ;
#6738 = DIRECTION ( 'NONE',  ( 0.000000000000000000, 0.000000000000000000, 1.000000000000000000 ) ) ;
#6739 = EDGE_LOOP ( 'NONE', ( #416, #393, #6377, #903 ) ) ;
#6740 = VERTEX_POINT ( 'NONE', #4512 ) ;
#6741 = DIRECTION ( 'NONE',  ( -1.000000000000000000, 0.000000000000000000, 0.000000000000000000 ) ) ;
#6742 = CARTESIAN_POINT ( 'NONE',  ( -27.98076211353308551, 54.60416666475470038, -6.154700538379338504 ) ) ;
#6743 = CARTESIAN_POINT ( 'NONE',  ( 21.05771646464872404, 22.57981893131178452, 12.00579112326941988 ) ) ;
#6744 = DIRECTION ( 'NONE',  ( 1.000000000000000000, -0.000000000000000000, 1.156482317317871478E-16 ) ) ;
#6745 = EDGE_CURVE ( 'NONE', #9904, #2222, #1559, .T. ) ;
#6746 = DIRECTION ( 'NONE',  ( 0.000000000000000000, 0.000000000000000000, 1.000000000000000000 ) ) ;
#6747 = CARTESIAN_POINT ( 'NONE',  ( -25.98076211353311393, 54.44374999904394485, -3.128098921329806714 ) ) ;
#6748 = EDGE_CURVE ( 'NONE', #7325, #8937, #10072, .T. ) ;
#6749 = CARTESIAN_POINT ( 'NONE',  ( 26.25045812061784289, 53.49999999999983658, 14.50000000000000000 ) ) ;
#6750 = CARTESIAN_POINT ( 'NONE',  ( -25.84608536423723635, 56.99999999999889866, -3.000000000000131450 ) ) ;
#6751 = LINE ( 'NONE', #3643, #4554 ) ;
#6752 = ORIENTED_EDGE ( 'NONE', *, *, #9498, .T. ) ;
#6753 = DIRECTION ( 'NONE',  ( 0.000000000000000000, 0.000000000000000000, 1.000000000000000000 ) ) ;
#6754 = CARTESIAN_POINT ( 'NONE',  ( -27.98076211353308551, 53.32083333142136894, -3.845299461620869330 ) ) ;
#6755 = CARTESIAN_POINT ( 'NONE',  ( -25.17020516978313083, 53.27708333237728056, -3.596074190997380349 ) ) ;
#6756 = CARTESIAN_POINT ( 'NONE',  ( 0.000000000000000000, 0.000000000000000000, 0.000000000000000000 ) ) ;
#6757 = AXIS2_PLACEMENT_3D ( 'NONE', #10859, #1697, #3249 ) ;
#6758 = LINE ( 'NONE', #1882, #6249 ) ;
#6759 = CARTESIAN_POINT ( 'NONE',  ( -23.98076211353314235, 50.84166666666652645, -3.845299461620867554 ) ) ;
#6760 = ORIENTED_EDGE ( 'NONE', *, *, #2480, .T. ) ;
#6761 = ORIENTED_EDGE ( 'NONE', *, *, #10105, .F. ) ;
#6762 = VERTEX_POINT ( 'NONE', #3782 ) ;
#6763 = CYLINDRICAL_SURFACE ( 'NONE', #5046, 2.149999999999988809 ) ;
#6764 = ORIENTED_EDGE ( 'NONE', *, *, #5137, .F. ) ;
#6765 = DIRECTION ( 'NONE',  ( -0.7071067811865292541, 0.000000000000000000, 0.7071067811865657804 ) ) ;
#6766 = CARTESIAN_POINT ( 'NONE',  ( -1.734723475976807094E-14, 3.469446951953614189E-15, 5.000000000000009770 ) ) ;
#6767 = AXIS2_PLACEMENT_3D ( 'NONE', #3029, #6403, #10475 ) ;
#6768 = ORIENTED_EDGE ( 'NONE', *, *, #7713, .F. ) ;
#6769 = CARTESIAN_POINT ( 'NONE',  ( 19.09861202765586086, 17.13671095651997689, 11.00988473025352121 ) ) ;
#6770 = CARTESIAN_POINT ( 'NONE',  ( 24.30992024302469900, 5.833333333333329485, -2.500000000000000000 ) ) ;
#6771 = DIRECTION ( 'NONE',  ( 0.000000000000000000, 0.000000000000000000, 1.000000000000000000 ) ) ;
#6772 = CARTESIAN_POINT ( 'NONE',  ( -25.98076211353311393, 49.49999999999986500, -7.000000000000074607 ) ) ;
#6773 = CARTESIAN_POINT ( 'NONE',  ( 20.62599888145302529, 16.93661977612163128, 10.95195840513859231 ) ) ;
#6774 = EDGE_CURVE ( 'NONE', #10496, #5165, #3010, .T. ) ;
#6775 = CARTESIAN_POINT ( 'NONE',  ( 2.100000000000000089, 0.000000000000000000, -5.000000000000000000 ) ) ;
#6776 = CARTESIAN_POINT ( 'NONE',  ( -25.98076211353311393, 51.11874999904394201, -3.128098921329806714 ) ) ;
#6777 = DIRECTION ( 'NONE',  ( 0.000000000000000000, -0.000000000000000000, -1.000000000000000000 ) ) ;
#6778 = VERTEX_POINT ( 'NONE', #5669 ) ;
#6779 = CARTESIAN_POINT ( 'NONE',  ( -25.98076211353311393, 49.49999999999986500, -7.000000000000074607 ) ) ;
#6780 = PRODUCT_DEFINITION_SHAPE ( 'NONE', 'NONE',  #8571 ) ;
#6781 = ORIENTED_EDGE ( 'NONE', *, *, #2738, .F. ) ;
#6782 = CARTESIAN_POINT ( 'NONE',  ( 3.500000000000005773, 31.44974746830583356, 15.92187500000000178 ) ) ;
#6783 = AXIS2_PLACEMENT_3D ( 'NONE', #2607, #3492, #10208 ) ;
#6784 = ORIENTED_EDGE ( 'NONE', *, *, #6189, .F. ) ;
#6785 = CARTESIAN_POINT ( 'NONE',  ( 23.09245737654782360, 19.89859478643763069, 13.00425721518307753 ) ) ;
#6786 = CARTESIAN_POINT ( 'NONE',  ( 16.19085831639981166, 17.34467558953214095, 12.14735994959122856 ) ) ;
#6787 = CARTESIAN_POINT ( 'NONE',  ( 23.13231036272843966, 20.08340223762181154, 12.00579112326941988 ) ) ;
#6788 = CARTESIAN_POINT ( 'NONE',  ( -24.35964822603314772, 52.57708333237728482, -5.935950539335252074 ) ) ;
#6789 = CARTESIAN_POINT ( 'NONE',  ( 4.553649124439118623E-15, 27.49999999999999289, 15.53125000000000355 ) ) ;
#6790 = FACE_BOUND ( 'NONE', #10633, .T. ) ;
#6791 = DIRECTION ( 'NONE',  ( -0.000000000000000000, 0.000000000000000000, -1.000000000000000000 ) ) ;
#6792 = DIRECTION ( 'NONE',  ( 1.000000000000000000, 0.000000000000000000, 0.000000000000000000 ) ) ;
#6793 = ORIENTED_EDGE ( 'NONE', *, *, #5666, .T. ) ;
#6794 = ORIENTED_EDGE ( 'NONE', *, *, #1624, .T. ) ;
#6795 = ADVANCED_BREP_SHAPE_REPRESENTATION ( '', ( #5559, #308 ), #5109 ) ;
#6796 = CARTESIAN_POINT ( 'NONE',  ( 2.000000000000005329, -3.464101615137751722, 0.000000000000000000 ) ) ;
#6797 = CARTESIAN_POINT ( 'NONE',  ( -1.219727444046192735E-16, 2.000000000000000000, -5.500000000000000000 ) ) ;
#6798 = CARTESIAN_POINT ( 'NONE',  ( 18.62184541094303114, 16.98042197548449295, 12.02177981800743112 ) ) ;
#6799 = ADVANCED_FACE ( 'NONE', ( #3888 ), #7594, .F. ) ;
#6800 = DIRECTION ( 'NONE',  ( 0.000000000000000000, 0.000000000000000000, 1.000000000000000000 ) ) ;
#6801 = CARTESIAN_POINT ( 'NONE',  ( -24.35964822603314417, 52.51874999904394770, -5.000000000000103029 ) ) ;
#6802 = DIRECTION ( 'NONE',  ( -0.000000000000000000, -0.000000000000000000, -1.000000000000000000 ) ) ;
#6803 = CARTESIAN_POINT ( 'NONE',  ( 29.49999999999999645, -8.499999999999985789, -4.999999999999991118 ) ) ;
#6804 = VERTEX_POINT ( 'NONE', #8323 ) ;
#6805 = DIRECTION ( 'NONE',  ( 0.000000000000000000, 0.000000000000000000, -1.000000000000000000 ) ) ;
#6806 = DIRECTION ( 'NONE',  ( 1.000000000000000000, 0.000000000000000000, 0.000000000000000000 ) ) ;
#6807 = EDGE_CURVE ( 'NONE', #5318, #2956, #3651, .T. ) ;
#6808 = CARTESIAN_POINT ( 'NONE',  ( -27.60187600103308370, 54.44374999904394485, -5.000000000000103029 ) ) ;
#6809 = CONICAL_SURFACE ( 'NONE', #591, 2.055000000000000160, 0.7853981633974721488 ) ;
#6810 = CARTESIAN_POINT ( 'NONE',  ( 4.750000000000000888, -3.250000000000000444, -3.980102097228895766E-16 ) ) ;
#6811 = EDGE_CURVE ( 'NONE', #318, #1508, #9000, .T. ) ;
#6812 = CARTESIAN_POINT ( 'NONE',  ( 0.000000000000000000, 0.000000000000000000, -5.000000000000000888 ) ) ;
#6813 = CARTESIAN_POINT ( 'NONE',  ( -24.98076211353313170, 53.58333333333320070, -3.267949192431250705 ) ) ;
#6814 = AXIS2_PLACEMENT_3D ( 'NONE', #2195, #10649, #3869 ) ;
#6815 = VERTEX_POINT ( 'NONE', #4890 ) ;
#6816 = AXIS2_PLACEMENT_3D ( 'NONE', #3111, #6489, #3212 ) ;
#6817 = VERTEX_POINT ( 'NONE', #8163 ) ;
#6818 = CARTESIAN_POINT ( 'NONE',  ( -2.100000000000000089, 2.571758278209441957E-16, -4.694516984716113228 ) ) ;
#6819 = ORIENTED_EDGE ( 'NONE', *, *, #2127, .F. ) ;
#6820 = ADVANCED_FACE ( 'NONE', ( #10666 ), #8967, .F. ) ;
#6821 = CARTESIAN_POINT ( 'NONE',  ( 3.200000000000000178, -0.3416191432522810434, -3.499999999999999112 ) ) ;
#6822 = DIRECTION ( 'NONE',  ( 0.000000000000000000, 0.000000000000000000, 1.000000000000000000 ) ) ;
#6823 = ORIENTED_EDGE ( 'NONE', *, *, #3987, .F. ) ;
#6824 = DIRECTION ( 'NONE',  ( 0.000000000000000000, 0.000000000000000000, 1.000000000000000000 ) ) ;
#6825 = DIRECTION ( 'NONE',  ( -0.000000000000000000, -0.000000000000000000, -1.000000000000000000 ) ) ;
#6826 = AXIS2_PLACEMENT_3D ( 'NONE', #4109, #8908, #10882 ) ;
#6827 = DIRECTION ( 'NONE',  ( -0.000000000000000000, -0.000000000000000000, -1.000000000000000000 ) ) ;
#6828 =( BOUNDED_CURVE ( )  B_SPLINE_CURVE ( 2, ( #5950, #4172, #6727, #5072, #2507, #5894, #9279, #5181, #8508 ),
 .UNSPECIFIED., .F., .F. ) 
 B_SPLINE_CURVE_WITH_KNOTS ( ( 3, 2, 2, 2, 3 ),
 ( 0.02777777777777777971, 0.03703703703703703498, 0.05555555555555555247, 0.07407407407407406996, 0.08333333333333338422 ),
 .UNSPECIFIED. ) 
 CURVE ( )  GEOMETRIC_REPRESENTATION_ITEM ( )  RATIONAL_B_SPLINE_CURVE ( ( 0.9330127018922194093, 0.9330127018922194093, 1.000000000000000000, 0.8660254037844387076, 1.000000000000000000, 0.8660254037844387076, 1.000000000000000000, 0.9330127018922189652, 0.9330127018922194093 ) ) 
 REPRESENTATION_ITEM ( '' )  );
#6829 = AXIS2_PLACEMENT_3D ( 'NONE', #7606, #1664, #5061 ) ;
#6830 = CARTESIAN_POINT ( 'NONE',  ( -27.60187600103308370, 50.24374999904394912, -5.000000000000103029 ) ) ;
#6831 = EDGE_CURVE ( 'NONE', #9793, #10907, #805, .T. ) ;
#6832 = EDGE_CURVE ( 'NONE', #10839, #6057, #593, .T. ) ;
#6833 = CARTESIAN_POINT ( 'NONE',  ( 20.15426471261298147, 16.54100339847095213, 11.95042283504686154 ) ) ;
#6834 = CARTESIAN_POINT ( 'NONE',  ( 0.000000000000000000, 0.000000000000000000, 0.000000000000000000 ) ) ;
#6835 = CARTESIAN_POINT ( 'NONE',  ( -24.35964822603314772, 50.53541666571060631, -4.064049460664953983 ) ) ;
#6836 = AXIS2_PLACEMENT_3D ( 'NONE', #5698, #5803, #9867 ) ;
#6837 = CARTESIAN_POINT ( 'NONE',  ( -25.98076211353310683, 53.52499999999986358, -3.000000000000132339 ) ) ;
#6838 = VERTEX_POINT ( 'NONE', #4835 ) ;
#6839 = CARTESIAN_POINT ( 'NONE',  ( -25.36463575557657180, 58.79801918157050977, -3.094798637517150564 ) ) ;
#6840 = VERTEX_POINT ( 'NONE', #8211 ) ;
#6841 = CARTESIAN_POINT ( 'NONE',  ( 3.500000000000007994, 28.55025253169416644, 15.76562500000000178 ) ) ;
#6842 = AXIS2_PLACEMENT_3D ( 'NONE', #8969, #2092, #9858 ) ;
#6843 = ORIENTED_EDGE ( 'NONE', *, *, #3732, .T. ) ;
#6844 = CARTESIAN_POINT ( 'NONE',  ( 16.03488360227938969, 17.50065030365295016, 12.16198771834549497 ) ) ;
#6845 =( NAMED_UNIT ( * ) PLANE_ANGLE_UNIT ( ) SI_UNIT ( $, .RADIAN. ) );
#6846 = CARTESIAN_POINT ( 'NONE',  ( -25.10866622795798619, 58.50632701280146364, -6.800737734245783095 ) ) ;
#6847 = CARTESIAN_POINT ( 'NONE',  ( 23.31827848602400621, 20.57738196266585362, 12.00579112326941988 ) ) ;
#6849 = CARTESIAN_POINT ( 'NONE',  ( -24.35964822603314772, 52.46041666571062478, -4.064049460664953983 ) ) ;
#6848 = CIRCLE ( 'NONE', #9872, 0.5155456020628804703 ) ;
#6850 = CARTESIAN_POINT ( 'NONE',  ( 2.500000000000007550, 31.03553390593274486, 15.92187500000000178 ) ) ;
#6851 = DIRECTION ( 'NONE',  ( -0.000000000000000000, 1.000000000000000000, -0.000000000000000000 ) ) ;
#6852 = CARTESIAN_POINT ( 'NONE',  ( -26.77852525657794658, 58.61651288262306281, -6.836577306127424869 ) ) ;
#6853 = VERTEX_POINT ( 'NONE', #4051 ) ;
#6854 = EDGE_CURVE ( 'NONE', #9431, #6331, #4177, .T. ) ;
#6855 = ORIENTED_EDGE ( 'NONE', *, *, #10765, .F. ) ;
#6856 = DIRECTION ( 'NONE',  ( 0.000000000000000000, 0.000000000000000000, -1.000000000000000000 ) ) ;
#6857 = TOROIDAL_SURFACE ( 'NONE', #5445, 3.299999999999999822, 0.2000000000000000111 ) ;
#6858 = CARTESIAN_POINT ( 'NONE',  ( -4.000000000000000888, -1.539600717839011201, -3.300726591567081591 ) ) ;
#6859 = CARTESIAN_POINT ( 'NONE',  ( 34.85635190221861990, 3.172051726186627008, -3.113055717248542464 ) ) ;
#6860 = DIRECTION ( 'NONE',  ( -0.000000000000000000, 1.000000000000000000, 1.224646799147353207E-16 ) ) ;
#6861 = LINE ( 'NONE', #6973, #8352 ) ;
#6862 = CARTESIAN_POINT ( 'NONE',  ( -27.60187600103308014, 52.22708333237728340, -4.064049460664955760 ) ) ;
#6863 = SURFACE_STYLE_FILL_AREA ( #9365 ) ;
#6864 = CARTESIAN_POINT ( 'NONE',  ( 1.567478505476135000E-15, 4.618802153517012954, -3.504269196027527844 ) ) ;
#6865 = DIRECTION ( 'NONE',  ( 0.000000000000000000, 0.000000000000000000, 1.000000000000000000 ) ) ;
#6866 = ORIENTED_EDGE ( 'NONE', *, *, #2787, .T. ) ;
#6867 = CARTESIAN_POINT ( 'NONE',  ( 1.767766952966372429, 31.76776695296637598, 13.50000000000000355 ) ) ;
#6868 = ADVANCED_FACE ( 'NONE', ( #1490 ), #7021, .T. ) ;
#6869 = PRODUCT_DEFINITION_FORMATION_WITH_SPECIFIED_SOURCE ( 'ANY', '', #466, .NOT_KNOWN. ) ;
#6870 = CARTESIAN_POINT ( 'NONE',  ( 25.00000000000000000, 2.516649172247811061E-16, -2.055000000000000160 ) ) ;
#6871 = CARTESIAN_POINT ( 'NONE',  ( -26.79131905728310059, 52.92708333237727913, -6.403925809002825709 ) ) ;
#6872 = CARTESIAN_POINT ( 'NONE',  ( -23.98076211353314235, 50.89999999999986358, -5.000000000000103029 ) ) ;
#6873 = PRODUCT_DEFINITION_SHAPE ( 'NONE', 'NONE',  #11004 ) ;
#6874 = DIRECTION ( 'NONE',  ( 0.000000000000000000, 0.000000000000000000, -1.000000000000000000 ) ) ;
#6875 = CIRCLE ( 'NONE', #2095, 4.999999999999997335 ) ;
#6876 = CIRCLE ( 'NONE', #1554, 24.99999999999999645 ) ;
#6877 = CARTESIAN_POINT ( 'NONE',  ( -25.98076211353311393, 54.92499999999986926, -2.690598923241634743 ) ) ;
#6878 = ORIENTED_EDGE ( 'NONE', *, *, #2907, .F. ) ;
#6879 = ADVANCED_FACE ( 'NONE', ( #3989, #10825 ), #3209, .T. ) ;
#6880 = ORIENTED_EDGE ( 'NONE', *, *, #1517, .T. ) ;
#6881 = FACE_OUTER_BOUND ( 'NONE', #6730, .T. ) ;
#6882 = EDGE_CURVE ( 'NONE', #3061, #4045, #2006, .T. ) ;
#6883 = ADVANCED_FACE ( 'NONE', ( #9990 ), #701, .T. ) ;
#6884 = DIRECTION ( 'NONE',  ( 0.000000000000000000, 0.000000000000000000, 1.000000000000000000 ) ) ;
#6885 =( NAMED_UNIT ( * ) PLANE_ANGLE_UNIT ( ) SI_UNIT ( $, .RADIAN. ) );
#6886 = ORIENTED_EDGE ( 'NONE', *, *, #7702, .T. ) ;
#6888 = CARTESIAN_POINT ( 'NONE',  ( 19.55162244606592381, 17.33808635661342024, 12.00579012602852735 ) ) ;
#6887 = VECTOR ( 'NONE', #10395, 1000.000000000000000 ) ;
#6889 = STYLED_ITEM ( 'NONE', ( #5399 ), #1232 ) ;
#6890 = LINE ( 'NONE', #162, #2046 ) ;
#6891 = DIRECTION ( 'NONE',  ( -1.000000000000000000, 0.000000000000000000, 0.000000000000000000 ) ) ;
#6892 = VECTOR ( 'NONE', #3540, 1000.000000000000000 ) ;
#6893 = CARTESIAN_POINT ( 'NONE',  ( -24.35964822603314417, 54.09374999904395054, -5.000000000000103029 ) ) ;
#6894 = CARTESIAN_POINT ( 'NONE',  ( 23.22881793621964874, 18.67973499377871960, 11.95042449705234588 ) ) ;
#6895 = ADVANCED_FACE ( 'NONE', ( #5561 ), #8942, .T. ) ;
#6896 = ADVANCED_FACE ( 'NONE', ( #9888, #2278, #10994 ), #5932, .F. ) ;
#6897 = CARTESIAN_POINT ( 'NONE',  ( 0.000000000000000000, 0.000000000000000000, 3.299999999999999822 ) ) ;
#6898 = EDGE_CURVE ( 'NONE', #7216, #3459, #5401, .T. ) ;
#6899 = CARTESIAN_POINT ( 'NONE',  ( -25.98076211353311393, 54.83749999808803466, -2.690598923241634743 ) ) ;
#6900 = AXIS2_PLACEMENT_3D ( 'NONE', #6342, #2860, #5353 ) ;
#6901 = CARTESIAN_POINT ( 'NONE',  ( -25.44486372867087809, 53.84373926088289863, -7.000000000000075495 ) ) ;
#6902 = VERTEX_POINT ( 'NONE', #3325 ) ;
#6903 = CARTESIAN_POINT ( 'NONE',  ( -4.000000000000000000, -2.309401076758515803, -0.4999999999999995559 ) ) ;
#6904 = ORIENTED_EDGE ( 'NONE', *, *, #2996, .F. ) ;
#6905 = CARTESIAN_POINT ( 'NONE',  ( -3.500000000000001332, 29.93383077435482065, 14.22094158473306535 ) ) ;
#6906 = ORIENTED_EDGE ( 'NONE', *, *, #9474, .T. ) ;
#6907 = CARTESIAN_POINT ( 'NONE',  ( 18.83541841558448837, 19.97999999654625825, 12.94889058896590583 ) ) ;
#6908 = CARTESIAN_POINT ( 'NONE',  ( 20.26791470906062997, 16.62008925861079334, 11.95042449705224819 ) ) ;
#6909 = CARTESIAN_POINT ( 'NONE',  ( 22.69616945897178084, 19.53356342368596898, 12.00579112326941988 ) ) ;
#6910 = CARTESIAN_POINT ( 'NONE',  ( -24.35964822603314772, 49.77708333237728766, -5.935950539335252074 ) ) ;
#6911 = DIRECTION ( 'NONE',  ( 0.000000000000000000, 0.000000000000000000, 1.000000000000000000 ) ) ;
#6912 = DIRECTION ( 'NONE',  ( -1.000000000000000000, -0.000000000000000000, -0.000000000000000000 ) ) ;
#6913 = CARTESIAN_POINT ( 'NONE',  ( -25.98076211353311393, 51.42499999999986926, -3.000000000000132783 ) ) ;
#6914 = ORIENTED_EDGE ( 'NONE', *, *, #6607, .F. ) ;
#6915 = VERTEX_POINT ( 'NONE', #4275 ) ;
#6916 = CARTESIAN_POINT ( 'NONE',  ( 18.79784185921769790, 16.99560944861731215, 12.01584860934582366 ) ) ;
#6917 = CARTESIAN_POINT ( 'NONE',  ( -3.049318610115481714E-16, 5.000000000000000000, -2.500000000000000000 ) ) ;
#6918 = CARTESIAN_POINT ( 'NONE',  ( 22.11805565807571128, 22.55986279155152374, 12.00579112326941988 ) ) ;
#6919 = CARTESIAN_POINT ( 'NONE',  ( -25.98076211353311038, 57.99999999999985789, -9.000000000000701661 ) ) ;
#6920 = CARTESIAN_POINT ( 'NONE',  ( 4.175002511812151873, 2.208363329454889445, -3.469254087858244073 ) ) ;
#6921 = CARTESIAN_POINT ( 'NONE',  ( -25.98076211353311393, 51.99374999904394912, -6.871901078670400231 ) ) ;
#6922 = CARTESIAN_POINT ( 'NONE',  ( 19.86292016999849608, 19.38279280778333202, 11.97810781016083403 ) ) ;
#6923 = CARTESIAN_POINT ( 'NONE',  ( 2.000000000000005329, -3.464101615137751722, 0.000000000000000000 ) ) ;
#6924 = LINE ( 'NONE', #5317, #8089 ) ;
#6925 = ADVANCED_FACE ( 'NONE', ( #1716 ), #3264, .F. ) ;
#6926 = VERTEX_POINT ( 'NONE', #6713 ) ;
#6927 = FACE_OUTER_BOUND ( 'NONE', #4411, .T. ) ;
#6928 = CARTESIAN_POINT ( 'NONE',  ( -0.9693646802875689472, 32.52740819067395961, 17.23218341526694530 ) ) ;
#6929 = CARTESIAN_POINT ( 'NONE',  ( -1.767766952966375094, 31.76776695296636888, 15.06250000000000355 ) ) ;
#6930 = CARTESIAN_POINT ( 'NONE',  ( -25.17020516978313083, 54.67708333237727913, -3.596074190997380349 ) ) ;
#6931 = CARTESIAN_POINT ( 'NONE',  ( -25.98076211353310683, 54.92499999999986926, -3.000000000000132339 ) ) ;
#6932 = DIRECTION ( 'NONE',  ( 0.000000000000000000, 1.000000000000000000, 0.000000000000000000 ) ) ;
#6933 = DIRECTION ( 'NONE',  ( 1.000000000000000000, -0.000000000000000000, -0.000000000000000000 ) ) ;
#6934 = VERTEX_POINT ( 'NONE', #6818 ) ;
#6935 = ORIENTED_EDGE ( 'NONE', *, *, #740, .F. ) ;
#6936 = DIRECTION ( 'NONE',  ( 1.000000000000000000, 6.098637220230963674E-17, 0.000000000000000000 ) ) ;
#6937 = DIRECTION ( 'NONE',  ( -0.000000000000000000, -0.000000000000000000, 1.000000000000000000 ) ) ;
#6938 = APPLICATION_PROTOCOL_DEFINITION ( 'draft international standard', 'automotive_design', 1998, #7412 ) ;
#6939 = ORIENTED_EDGE ( 'NONE', *, *, #9838, .T. ) ;
#6940 = CARTESIAN_POINT ( 'NONE',  ( 29.50000000000000711, 2.000000000000001776, -12.50000000000000000 ) ) ;
#6941 = VECTOR ( 'NONE', #7588, 1000.000000000000000 ) ;
#6942 = DIRECTION ( 'NONE',  ( -0.000000000000000000, -0.000000000000000000, 1.000000000000000000 ) ) ;
#6943 = B_SPLINE_CURVE_WITH_KNOTS ( 'NONE', 3,
 ( #7621, #2454, #6663, #2627, #9222, #6725 ),
 .UNSPECIFIED., .F., .F.,
 ( 4, 2, 4 ),
 ( 0.002452478801916376308, 0.003676905084148007850, 0.004901331366379639391 ),
 .UNSPECIFIED. ) ;
#6944 = CARTESIAN_POINT ( 'NONE',  ( 18.90462188152790901, 16.04371289204410189, 10.96879988954262153 ) ) ;
#6945 = DIRECTION ( 'NONE',  ( -0.000000000000000000, -0.000000000000000000, -1.000000000000000000 ) ) ;
#6946 = CARTESIAN_POINT ( 'NONE',  ( -24.35964822603314417, 53.39374999904394770, -5.000000000000103029 ) ) ;
#6947 = AXIS2_PLACEMENT_3D ( 'NONE', #9456, #4246, #1745 ) ;
#6948 = CARTESIAN_POINT ( 'NONE',  ( 30.75045812061784289, 56.49999999999984368, 10.00000000000000178 ) ) ;
#6949 = ORIENTED_EDGE ( 'NONE', *, *, #7569, .T. ) ;
#6950 = AXIS2_PLACEMENT_3D ( 'NONE', #2680, #6056, #7502 ) ;
#6951 = DIRECTION ( 'NONE',  ( -1.000000000000000000, -6.098637220230963674E-17, 0.000000000000000000 ) ) ;
#6952 = VERTEX_POINT ( 'NONE', #39 ) ;
#6953 = CARTESIAN_POINT ( 'NONE',  ( 2.474873734152922111, 27.52512626584708144, 15.68750000000000355 ) ) ;
#6954 = EDGE_LOOP ( 'NONE', ( #3659, #3604, #10314, #4965, #1045 ) ) ;
#6955 = CARTESIAN_POINT ( 'NONE',  ( 16.65878245872646701, 16.87675144720473952, 12.10347664333366247 ) ) ;
#6956 = CARTESIAN_POINT ( 'NONE',  ( 0.000000000000000000, 0.000000000000000000, 0.000000000000000000 ) ) ;
#6957 = EDGE_CURVE ( 'NONE', #874, #10104, #6277, .T. ) ;
#6958 = CARTESIAN_POINT ( 'NONE',  ( 34.99999999999999289, -3.999999999999993339, -4.999999999999995559 ) ) ;
#6959 = CARTESIAN_POINT ( 'NONE',  ( 23.33980466280999977, 20.94445964013513617, 12.00579112326902909 ) ) ;
#6960 = CARTESIAN_POINT ( 'NONE',  ( -25.17020516978313083, 49.83541666571061768, -6.403925809002825709 ) ) ;
#6961 = LINE ( 'NONE', #2804, #3532 ) ;
#6962 = CIRCLE ( 'NONE', #10683, 2.149999999999992362 ) ;
#6963 = DIRECTION ( 'NONE',  ( 1.000000000000000000, 0.000000000000000000, 0.000000000000000000 ) ) ;
#6964 = FACE_OUTER_BOUND ( 'NONE', #9608, .T. ) ;
#6965 = ORIENTED_EDGE ( 'NONE', *, *, #1042, .F. ) ;
#6966 = VERTEX_POINT ( 'NONE', #8433 ) ;
#6967 = CARTESIAN_POINT ( 'NONE',  ( 0.02539999999999975264, 0.000000000000000000, -2.000000000000000000 ) ) ;
#6968 = EDGE_CURVE ( 'NONE', #6545, #6778, #8602, .T. ) ;
#6969 = PLANE ( 'NONE',  #3845 ) ;
#6970 = PRODUCT_DEFINITION_SHAPE ( 'NONE', 'NONE',  #11009 ) ;
#6971 = CIRCLE ( 'NONE', #2178, 4.500000000000000888 ) ;
#6972 = CYLINDRICAL_SURFACE ( 'NONE', #5433, 7.500000000000000000 ) ;
#6973 = CARTESIAN_POINT ( 'NONE',  ( 25.49999999999999645, -3.999999999999983569, 11.65000000000000746 ) ) ;
#6974 = CARTESIAN_POINT ( 'NONE',  ( -27.60187600103308014, 55.61041666571061626, -5.935950539335252074 ) ) ;
#6975 = ADVANCED_FACE ( 'NONE', ( #6881 ), #10051, .F. ) ;
#6976 =( NAMED_UNIT ( * ) PLANE_ANGLE_UNIT ( ) SI_UNIT ( $, .RADIAN. ) );
#6977 = CYLINDRICAL_SURFACE ( 'NONE', #2581, 1.999999999999971356 ) ;
#6978 = DIRECTION ( 'NONE',  ( -1.000000000000000000, 0.000000000000000000, 0.000000000000000000 ) ) ;
#6979 = ORIENTED_EDGE ( 'NONE', *, *, #8372, .F. ) ;
#6980 =( NAMED_UNIT ( * ) PLANE_ANGLE_UNIT ( ) SI_UNIT ( $, .RADIAN. ) );
#6981 = CARTESIAN_POINT ( 'NONE',  ( -1.035533905932736420, 27.49999999999998934, 15.45312500000000178 ) ) ;
#6982 = CARTESIAN_POINT ( 'NONE',  ( 1.767766952966377314, 28.23223304703363112, 15.68750000000000355 ) ) ;
#6983 = UNCERTAINTY_MEASURE_WITH_UNIT (LENGTH_MEASURE( 1.000000000000000082E-05 ), #3841, 'distance_accuracy_value', 'NONE');
#6984 = CARTESIAN_POINT ( 'NONE',  ( 0.000000000000000000, 0.000000000000000000, -25.03750572909317285 ) ) ;
#6985 = EDGE_CURVE ( 'NONE', #6272, #4377, #5880, .T. ) ;
#6986 = CARTESIAN_POINT ( 'NONE',  ( -24.98076211353312814, 55.21666666666653356, -6.732050807568954909 ) ) ;
#6987 = LINE ( 'NONE', #10372, #8564 ) ;
#6988 = CARTESIAN_POINT ( 'NONE',  ( 4.750000000000000888, -1.622657008870242882E-15, 0.000000000000000000 ) ) ;
#6989 = VERTEX_POINT ( 'NONE', #1828 ) ;
#6990 = ORIENTED_EDGE ( 'NONE', *, *, #1805, .T. ) ;
#6991 = CARTESIAN_POINT ( 'NONE',  ( 34.94281041931228771, 2.000000000000002220, -5.500000000000000000 ) ) ;
#6992 = CARTESIAN_POINT ( 'NONE',  ( 2.500000000000000000, 2.357898499370433054, -1.951563910473907981E-15 ) ) ;
#6993 = SHAPE_DEFINITION_REPRESENTATION ( #3849, #6402 ) ;
#6994 = ORIENTED_EDGE ( 'NONE', *, *, #7524, .F. ) ;
#6995 = AXIS2_PLACEMENT_3D ( 'NONE', #4141, #7595, #10038 ) ;
#6996 = LINE ( 'NONE', #10331, #4883 ) ;
#6997 = DIRECTION ( 'NONE',  ( -0.9396926207859138680, 0.000000000000000000, -0.3420201433256536139 ) ) ;
#6998 = CARTESIAN_POINT ( 'NONE',  ( 18.76105380172462844, 21.09515122317004909, 11.95042449705224819 ) ) ;
#6999 = AXIS2_PLACEMENT_3D ( 'NONE', #10772, #5830, #2326 ) ;
#7000 = CARTESIAN_POINT ( 'NONE',  ( -3.500000000000003997, 31.44974746830583001, 16.39062500000000355 ) ) ;
#7001 = CARTESIAN_POINT ( 'NONE',  ( -26.79131905728310059, 54.32708333237727771, -6.403925809002825709 ) ) ;
#7002 = CARTESIAN_POINT ( 'NONE',  ( 34.99999999999999289, -3.999999999999993339, -2.850000000000008082 ) ) ;
#7003 = EDGE_LOOP ( 'NONE', ( #3851, #8606 ) ) ;
#7004 = CARTESIAN_POINT ( 'NONE',  ( 2.121320343559645494, 32.12132034355964549, 13.50000000000000355 ) ) ;
#7005 = ORIENTED_EDGE ( 'NONE', *, *, #5734, .T. ) ;
#7006 = CARTESIAN_POINT ( 'NONE',  ( -2.385244779468109755E-15, 32.50000000000000711, 14.90625000000000355 ) ) ;
#7007 = AXIS2_PLACEMENT_3D ( 'NONE', #9467, #3587, #3636 ) ;
#7008 = VERTEX_POINT ( 'NONE', #2438 ) ;
#7009 = ADVANCED_FACE ( 'NONE', ( #4392 ), #6763, .F. ) ;
#7010 = CLOSED_SHELL ( 'NONE', ( #8664, #6478, #7690, #4742, #3040, #5568, #10473, #7525, #5794, #7156, #4721, #2266, #581, #2001, #6879, #10239, #9936, #709, #2771, #2716, #2699, #5849, #8860, #3248, #10688, #4656, #3361, #4047, #2573, #4600, #9333, #4535 ) ) ;
#7011 = CARTESIAN_POINT ( 'NONE',  ( 24.32342464814431438, 20.41340561598360992, 11.95042449705224996 ) ) ;
#7012 = AXIS2_PLACEMENT_3D ( 'NONE', #3099, #10040, #4827 ) ;
#7013 = CARTESIAN_POINT ( 'NONE',  ( 2.000000000000008882, 3.464101615137749945, 0.000000000000000000 ) ) ;
#7014 = CARTESIAN_POINT ( 'NONE',  ( 17.45361707773674809, 17.49611573659335662, 12.09524845743996657 ) ) ;
#7015 = CARTESIAN_POINT ( 'NONE',  ( -24.35964822603314772, 51.87708333237728908, -5.935950539335252074 ) ) ;
#7016 = VECTOR ( 'NONE', #8554, 1000.000000000000000 ) ;
#7017 = AXIS2_PLACEMENT_3D ( 'NONE', #2861, #9682, #9515 ) ;
#7018 = LINE ( 'NONE', #8736, #323 ) ;
#7019 = AXIS2_PLACEMENT_3D ( 'NONE', #2150, #8976, #1526 ) ;
#7020 = PRODUCT_RELATED_PRODUCT_CATEGORY ( 'part', '', ( #10340 ) ) ;
#7021 = CONICAL_SURFACE ( 'NONE', #10549, 3.500000000000591971, 0.7853981633974560506 ) ;
#7022 = PLANE ( 'NONE',  #7017 ) ;
#7023 = CARTESIAN_POINT ( 'NONE',  ( -25.98076211353311393, 53.08749999808803466, -7.000000000000072831 ) ) ;
#7024 = EDGE_CURVE ( 'NONE', #10270, #2599, #7252, .T. ) ;
#7025 = ORIENTED_EDGE ( 'NONE', *, *, #572, .T. ) ;
#7026 = ORIENTED_EDGE ( 'NONE', *, *, #2268, .F. ) ;
#7027 = ADVANCED_FACE ( 'NONE', ( #9209 ), #9263, .T. ) ;
#7028 = CARTESIAN_POINT ( 'NONE',  ( 16.89796509758404852, 18.05178237072099989, 12.14735994959144350 ) ) ;
#7029 = CIRCLE ( 'NONE', #1162, 4.000000000000000000 ) ;
#7030 = FACE_BOUND ( 'NONE', #9503, .T. ) ;
#7031 = VECTOR ( 'NONE', #3079, 1000.000000000000000 ) ;
#7032 = CARTESIAN_POINT ( 'NONE',  ( 26.17691601781025312, 59.99615088301337096, 2.500000000000000000 ) ) ;
#7033 = CARTESIAN_POINT ( 'NONE',  ( 0.000000000000000000, -1.178949249685213863, 2.042000000000002924 ) ) ;
#7034 = CARTESIAN_POINT ( 'NONE',  ( 21.21106610644839208, 56.49999999999984368, 10.00000000000000178 ) ) ;
#7035 = CARTESIAN_POINT ( 'NONE',  ( -25.98076211353311393, 49.49999999999986500, -7.000000000000074607 ) ) ;
#7036 = CARTESIAN_POINT ( 'NONE',  ( -1.734723475976807094E-15, 33.50000000000000000, 13.65625000000000355 ) ) ;
#7037 = CARTESIAN_POINT ( 'NONE',  ( 29.49999999999999289, 6.938893903907228378E-15, 17.50000000000000000 ) ) ;
#7038 = EDGE_CURVE ( 'NONE', #1951, #8894, #5000, .T. ) ;
#7039 = ORIENTED_EDGE ( 'NONE', *, *, #1262, .T. ) ;
#7040 =( LENGTH_UNIT ( ) NAMED_UNIT ( * ) SI_UNIT ( .MILLI., .METRE. ) );
#7041 = VECTOR ( 'NONE', #7305, 1000.000000000000114 ) ;
#7042 = CARTESIAN_POINT ( 'NONE',  ( 2.472591809326055046, 28.89829686842209355, 15.51343341526694353 ) ) ;
#7043 = CARTESIAN_POINT ( 'NONE',  ( -2.500000000000004885, 29.80321974748363090, 16.48359592357600434 ) ) ;
#7044 = DIRECTION ( 'NONE',  ( 0.000000000000000000, 0.000000000000000000, -1.000000000000000000 ) ) ;
#7045 = DIRECTION ( 'NONE',  ( -0.000000000000000000, 1.000000000000000000, -0.000000000000000000 ) ) ;
#7046 = B_SPLINE_CURVE_WITH_KNOTS ( 'NONE', 3,
 ( #3444, #6821, #8549, #4332, #755, #4155 ),
 .UNSPECIFIED., .F., .F.,
 ( 4, 2, 4 ),
 ( 0.01103649464086220618, 0.01205977283736834466, 0.01308305103387448487 ),
 .UNSPECIFIED. ) ;
#7047 = AXIS2_PLACEMENT_3D ( 'NONE', #8482, #8540, #1648 ) ;
#7048 = DIRECTION ( 'NONE',  ( -1.000000000000000000, -0.000000000000000000, -0.000000000000000000 ) ) ;
#7049 = DIRECTION ( 'NONE',  ( 0.000000000000000000, 1.000000000000000000, 0.000000000000000000 ) ) ;
#7050 = EDGE_LOOP ( 'NONE', ( #5017, #8548, #5250, #8139 ) ) ;
#7051 = CARTESIAN_POINT ( 'NONE',  ( -2.963055325167751164, 29.53063538693776735, 16.49922112211940117 ) ) ;
#7052 = ORIENTED_EDGE ( 'NONE', *, *, #3291, .F. ) ;
#7053 = DIRECTION ( 'NONE',  ( 0.000000000000000000, 0.000000000000000000, 1.000000000000000000 ) ) ;
#7054 = CARTESIAN_POINT ( 'NONE',  ( 6.098637220230963427E-16, -10.00000000000000000, -10.50000000000001243 ) ) ;
#7055 = SHAPE_DEFINITION_REPRESENTATION ( #9791, #5757 ) ;
#7056 = ORIENTED_EDGE ( 'NONE', *, *, #7861, .F. ) ;
#7057 = DIRECTION ( 'NONE',  ( -1.000000000000000000, 0.000000000000000000, -0.000000000000000000 ) ) ;
#7058 = CARTESIAN_POINT ( 'NONE',  ( -25.98076211353324894, 14.99999999999984190, -2.500000000000000000 ) ) ;
#7059 = AXIS2_PLACEMENT_3D ( 'NONE', #1982, #4541, #2302 ) ;
#7060 = CARTESIAN_POINT ( 'NONE',  ( 15.83366986443827962, 19.11607760386789323, 11.24497629747462568 ) ) ;
#7061 = CARTESIAN_POINT ( 'NONE',  ( 0.02539999999999975264, 0.000000000000000000, 0.000000000000000000 ) ) ;
#7062 = CARTESIAN_POINT ( 'NONE',  ( -25.17020516978313083, 53.97708333237728340, -3.596074190997380349 ) ) ;
#7063 = DIRECTION ( 'NONE',  ( 0.000000000000000000, 0.000000000000000000, 1.000000000000000000 ) ) ;
#7064 = EDGE_LOOP ( 'NONE', ( #2737, #3462, #8468, #2974 ) ) ;
#7065 = CARTESIAN_POINT ( 'NONE',  ( -30.98076211353325249, 14.99999999999984190, 2.500000000000000000 ) ) ;
#7066 = PRODUCT ( 'Cable Pinch Bolt Clamp', 'Cable Pinch Bolt Clamp', '', ( #160 ) ) ;
#7067 = ORIENTED_EDGE ( 'NONE', *, *, #4536, .T. ) ;
#7068 = CIRCLE ( 'NONE', #2271, 2.149999999999987921 ) ;
#7069 = CARTESIAN_POINT ( 'NONE',  ( -2.385244779468109755E-15, 32.50000000000000711, 13.65625000000000355 ) ) ;
#7070 = EDGE_LOOP ( 'NONE', ( #9225, #6949, #2780, #4661 ) ) ;
#7071 = CARTESIAN_POINT ( 'NONE',  ( 15.64372318925989802, 17.89181071667436385, 12.19867189564230969 ) ) ;
#7072 = SURFACE_SIDE_STYLE ('',( #7905 ) ) ;
#7073 = CARTESIAN_POINT ( 'NONE',  ( 25.49999999999999645, -3.999999999999983569, 10.00000000000000888 ) ) ;
#7074 = PRESENTATION_LAYER_ASSIGNMENT (  '', '', ( #9019 ) ) ;
#7075 = CARTESIAN_POINT ( 'NONE',  ( 19.80390141066272491, 20.29503604781401904, 13.00425721518307753 ) ) ;
#7076 = CARTESIAN_POINT ( 'NONE',  ( -24.35964822603314772, 53.27708333237728056, -5.935950539335252074 ) ) ;
#7077 = MECHANICAL_DESIGN_GEOMETRIC_PRESENTATION_REPRESENTATION (  '', ( #855 ), #7420 ) ;
#7078 = DIRECTION ( 'NONE',  ( 0.000000000000000000, 0.000000000000000000, 1.000000000000000000 ) ) ;
#7079 = CARTESIAN_POINT ( 'NONE',  ( -3.680118525130244400, 2.494084732383327285, -0.3507732604232449702 ) ) ;
#7080 = CYLINDRICAL_SURFACE ( 'NONE', #1742, 3.249999999999998224 ) ;
#7081 = ORIENTED_EDGE ( 'NONE', *, *, #5685, .F. ) ;
#7082 = FACE_OUTER_BOUND ( 'NONE', #8394, .T. ) ;
#7083 = DIRECTION ( 'NONE',  ( 1.000000000000000000, 0.000000000000000000, 0.000000000000000000 ) ) ;
#7084 = SURFACE_SIDE_STYLE ('',( #7922 ) ) ;
#7085 = CARTESIAN_POINT ( 'NONE',  ( 2.500000000000000000, -1.178949249685213863, 2.042000000000002924 ) ) ;
#7086 = DIRECTION ( 'NONE',  ( 0.000000000000000000, 0.000000000000000000, -1.000000000000000000 ) ) ;
#7087 = DIRECTION ( 'NONE',  ( 1.000000000000000000, 0.000000000000000000, 0.000000000000000000 ) ) ;
#7088 = CARTESIAN_POINT ( 'NONE',  ( 1.449747468305833120, 33.50000000000000000, 13.57812500000000178 ) ) ;
#7089 = CARTESIAN_POINT ( 'NONE',  ( 29.50000000000000711, 1.000000000000000888, -11.50000000000000711 ) ) ;
#7090 = VERTEX_POINT ( 'NONE', #3384 ) ;
#7091 = CARTESIAN_POINT ( 'NONE',  ( 34.99999999999999289, 2.000000000000002220, -12.49999999999999822 ) ) ;
#7092 = CARTESIAN_POINT ( 'NONE',  ( 2.500000000000009770, 29.93383077435482420, 15.59155841526693997 ) ) ;
#7093 = CARTESIAN_POINT ( 'NONE',  ( -2.500000000000007550, 31.03553390593274486, 13.89062500000000355 ) ) ;
#7094 = CARTESIAN_POINT ( 'NONE',  ( 19.85760542366876535, 20.31250532737884384, 12.00579112326941988 ) ) ;
#7095 = CARTESIAN_POINT ( 'NONE',  ( -23.98076211353314235, 55.07083333142136894, -6.154700538379337615 ) ) ;
#7096 = EDGE_CURVE ( 'NONE', #4107, #10330, #5198, .T. ) ;
#7097 = DIRECTION ( 'NONE',  ( 0.000000000000000000, -0.5000000000000011102, -0.8660254037844379305 ) ) ;
#7098 = EDGE_CURVE ( 'NONE', #7995, #1715, #9656, .T. ) ;
#7099 = CARTESIAN_POINT ( 'NONE',  ( -27.60187600103308014, 54.38541666571060773, -5.935950539335252074 ) ) ;
#7100 = LINE ( 'NONE', #8041, #10857 ) ;
#7101 = CARTESIAN_POINT ( 'NONE',  ( -25.98076211353311393, 54.57499999999985363, -7.309401076758571314 ) ) ;
#7102 = VERTEX_POINT ( 'NONE', #812 ) ;
#7103 = VERTEX_POINT ( 'NONE', #5329 ) ;
#7104 = CARTESIAN_POINT ( 'NONE',  ( 3.200000000000000178, 2.020725942163738686, 3.499999999999999556 ) ) ;
#7105 = LINE ( 'NONE', #2049, #9839 ) ;
#7106 = VERTEX_POINT ( 'NONE', #6991 ) ;
#7107 = CARTESIAN_POINT ( 'NONE',  ( -27.78269167149760577, 55.70378148983614608, -4.132215540378284757 ) ) ;
#7108 = ADVANCED_FACE ( 'NONE', ( #319 ), #6809, .T. ) ;
#7109 = LINE ( 'NONE', #2116, #8423 ) ;
#7110 = CARTESIAN_POINT ( 'NONE',  ( 17.54702143963720928, 17.40274154661815587, 11.08429399133878057 ) ) ;
#7111 = ORIENTED_EDGE ( 'NONE', *, *, #6530, .T. ) ;
#7112 = CARTESIAN_POINT ( 'NONE',  ( -24.35964822603314772, 54.15208333237728766, -5.935950539335252074 ) ) ;
#7113 = EDGE_LOOP ( 'NONE', ( #4126, #2126 ) ) ;
#7114 = CARTESIAN_POINT ( 'NONE',  ( 0.2176891316980006652, -1.691919446222015067, 3.500000000000000444 ) ) ;
#7115 = ORIENTED_EDGE ( 'NONE', *, *, #8949, .F. ) ;
#7116 = CARTESIAN_POINT ( 'NONE',  ( -1.035533905932736420, 27.49999999999998934, 14.20312500000000355 ) ) ;
#7117 = VERTEX_POINT ( 'NONE', #7831 ) ;
#7118 = CARTESIAN_POINT ( 'NONE',  ( 22.44460225903107187, 18.20165426066020942, 10.95195840513859231 ) ) ;
#7119 = ADVANCED_FACE ( 'NONE', ( #2723, #1269 ), #262, .T. ) ;
#7120 = DIRECTION ( 'NONE',  ( -0.7071067811865479058, -0.7071067811865470176, 0.000000000000000000 ) ) ;
#7121 = CARTESIAN_POINT ( 'NONE',  ( 19.72936730704260810, 17.39430066254168139, 13.00425721518307576 ) ) ;
#7122 = CARTESIAN_POINT ( 'NONE',  ( -27.60187600103308370, 55.69181177612239253, -4.629976868092589903 ) ) ;
#7123 = CIRCLE ( 'NONE', #10843, 7.500000000000000000 ) ;
#7124 = CARTESIAN_POINT ( 'NONE',  ( 24.49999999999999289, -6.767949192431108152, -4.999999999999992006 ) ) ;
#7125 = LINE ( 'NONE', #1237, #6120 ) ;
#7126 = LINE ( 'NONE', #9572, #10260 ) ;
#7127 = VERTEX_POINT ( 'NONE', #6154 ) ;
#7128 = ORIENTED_EDGE ( 'NONE', *, *, #6811, .T. ) ;
#7129 = FACE_OUTER_BOUND ( 'NONE', #971, .T. ) ;
#7130 = DIRECTION ( 'NONE',  ( 0.000000000000000000, 1.000000000000000000, 0.000000000000000000 ) ) ;
#7131 =( NAMED_UNIT ( * ) PLANE_ANGLE_UNIT ( ) SI_UNIT ( $, .RADIAN. ) );
#7132 = CYLINDRICAL_SURFACE ( 'NONE', #4181, 2.000000000000000000 ) ;
#7133 = CARTESIAN_POINT ( 'NONE',  ( 1.999999999999998224, -3.464101615137772594, -3.142992957459239012 ) ) ;
#7134 = CARTESIAN_POINT ( 'NONE',  ( -27.44132332507749794, 55.71836679508493262, -4.296600267573891685 ) ) ;
#7135 = DIRECTION ( 'NONE',  ( -0.000000000000000000, 1.000000000000000000, -0.000000000000000000 ) ) ;
#7136 = CARTESIAN_POINT ( 'NONE',  ( -3.500000000000003553, 31.44974746830583356, 15.14062500000000355 ) ) ;
#7137 = CARTESIAN_POINT ( 'NONE',  ( 1.411581201560190495E-15, 4.862606272033091592, -3.745885042887436622 ) ) ;
#7138 = ORIENTED_EDGE ( 'NONE', *, *, #8318, .T. ) ;
#7139 = CARTESIAN_POINT ( 'NONE',  ( -25.98076211353311038, 49.67499999999986215, -7.000000000000072831 ) ) ;
#7140 = CARTESIAN_POINT ( 'NONE',  ( 1.720978244806812496, 28.18544433887406342, 16.68530841526694175 ) ) ;
#7141 = CARTESIAN_POINT ( 'NONE',  ( 4.204015924366189871, -1.626724848190933548, -3.610627190413393084 ) ) ;
#7142 = TOROIDAL_SURFACE ( 'NONE', #8201, 2.700000000000001066, 0.2000000000000000111 ) ;
#7143 = CARTESIAN_POINT ( 'NONE',  ( 22.11805565807571128, 22.55986279155152374, 12.00579112326941988 ) ) ;
#7144 = EDGE_CURVE ( 'NONE', #10879, #6740, #2349, .T. ) ;
#7145 = DIRECTION ( 'NONE',  ( 6.098637220230963674E-17, -1.000000000000000000, 0.000000000000000000 ) ) ;
#7146 = DIRECTION ( 'NONE',  ( -1.000000000000000000, -0.000000000000000000, -0.000000000000000000 ) ) ;
#7147 = CARTESIAN_POINT ( 'NONE',  ( 24.49999999999999289, -1.232050807568863426, -4.999999999999992006 ) ) ;
#7148 = CARTESIAN_POINT ( 'NONE',  ( -25.98076211353311393, 51.81874999904394485, -3.128098921329806714 ) ) ;
#7149 = PRODUCT_DEFINITION_SHAPE ( 'NONE', 'NONE',  #7765 ) ;
#7150 = CYLINDRICAL_SURFACE ( 'NONE', #2526, 1.649999999999994360 ) ;
#7151 = VERTEX_POINT ( 'NONE', #3660 ) ;
#7152 = CARTESIAN_POINT ( 'NONE',  ( -25.98076211353311393, 49.49999999999986500, -5.000000000000103029 ) ) ;
#7153 = EDGE_CURVE ( 'NONE', #7117, #2061, #5750, .T. ) ;
#7154 = CARTESIAN_POINT ( 'NONE',  ( 29.49999999999999645, 1.000000000000004441, -11.50000000000000533 ) ) ;
#7155 = EDGE_LOOP ( 'NONE', ( #9714, #7327, #4427, #1816 ) ) ;
#7156 = ADVANCED_FACE ( 'NONE', ( #10378 ), #8712, .F. ) ;
#7157 = CARTESIAN_POINT ( 'NONE',  ( -0.6666666666666666297, -4.233901974057276973, -3.300726591567087365 ) ) ;
#7158 = DIRECTION ( 'NONE',  ( 1.156482317317871478E-16, -0.000000000000000000, -1.000000000000000000 ) ) ;
#7159 = CARTESIAN_POINT ( 'NONE',  ( 19.09861202765586086, 17.13671095651997689, 11.00988473025352121 ) ) ;
#7160 = ORIENTED_EDGE ( 'NONE', *, *, #1408, .T. ) ;
#7161 = CARTESIAN_POINT ( 'NONE',  ( -24.35964822603314772, 52.05208333237727913, -5.935950539335252074 ) ) ;
#7162 = EDGE_CURVE ( 'NONE', #6093, #3608, #6051, .T. ) ;
#7163 = ORIENTED_EDGE ( 'NONE', *, *, #5137, .T. ) ;
#7164 = CARTESIAN_POINT ( 'NONE',  ( 24.49999999999999289, 0.5000000000000159872, 10.00000000000000888 ) ) ;
#7165 = ORIENTED_EDGE ( 'NONE', *, *, #4850, .T. ) ;
#7166 = CARTESIAN_POINT ( 'NONE',  ( -1.101703131577916883, 32.47259180932605460, 12.73656658473306358 ) ) ;
#7167 = EDGE_LOOP ( 'NONE', ( #7543, #6728, #3740 ) ) ;
#7168 = CARTESIAN_POINT ( 'NONE',  ( 17.22114890795359798, 16.40384437412513208, 11.05348780010051435 ) ) ;
#7169 = EDGE_CURVE ( 'NONE', #3195, #3312, #5440, .T. ) ;
#7170 = EDGE_CURVE ( 'NONE', #1493, #7309, #9593, .T. ) ;
#7171 = AXIS2_PLACEMENT_3D ( 'NONE', #2365, #8202, #8987 ) ;
#7172 = CARTESIAN_POINT ( 'NONE',  ( 21.34179237787287065, 23.66094220255952152, 11.95042449705224819 ) ) ;
#7173 = CARTESIAN_POINT ( 'NONE',  ( 18.65992412991285221, 16.93717640447601269, 13.02011930655217675 ) ) ;
#7174 = CARTESIAN_POINT ( 'NONE',  ( 0.000000000000000000, 0.000000000000000000, 0.000000000000000000 ) ) ;
#7175 = AXIS2_PLACEMENT_3D ( 'NONE', #346, #238, #2866 ) ;
#7176 = CARTESIAN_POINT ( 'NONE',  ( -23.98076211353314235, 50.17083333142137036, -6.154700538379337615 ) ) ;
#7177 = CARTESIAN_POINT ( 'NONE',  ( -23.98076211353314235, 52.85416666475470038, -3.845299461620867554 ) ) ;
#7178 = ORIENTED_EDGE ( 'NONE', *, *, #5671, .T. ) ;
#7179 = CIRCLE ( 'NONE', #6816, 2.041999999999999815 ) ;
#7180 = ORIENTED_EDGE ( 'NONE', *, *, #4683, .F. ) ;
#7181 = CARTESIAN_POINT ( 'NONE',  ( 19.58285320134683261, 17.29236643726018130, 13.00425622583864715 ) ) ;
#7182 = DIRECTION ( 'NONE',  ( -1.156482317317871478E-16, 1.807003620809174139E-16, 1.000000000000000000 ) ) ;
#7183 = TOROIDAL_SURFACE ( 'NONE', #2765, 4.000000000000000000, 0.2500000000000000000 ) ;
#7184 = FACE_OUTER_BOUND ( 'NONE', #6592, .T. ) ;
#7185 = CARTESIAN_POINT ( 'NONE',  ( -25.98076211353311038, 49.67499999999986215, -7.000000000000072831 ) ) ;
#7186 =( BOUNDED_CURVE ( )  B_SPLINE_CURVE ( 2, ( #8310, #9422, #2661, #9305, #4939, #1647, #10984, #5979, #8417 ),
 .UNSPECIFIED., .F., .F. ) 
 B_SPLINE_CURVE_WITH_KNOTS ( ( 3, 2, 2, 2, 3 ),
 ( 0.1388888888888888951, 0.1481481481481481399, 0.1666666666666666574, 0.1851851851851851749, 0.1944444444444444475 ),
 .UNSPECIFIED. ) 
 CURVE ( )  GEOMETRIC_REPRESENTATION_ITEM ( )  RATIONAL_B_SPLINE_CURVE ( ( 0.9330127018922192983, 0.9330127018922194093, 1.000000000000000000, 0.8660254037844387076, 1.000000000000000000, 0.8660254037844387076, 1.000000000000000000, 0.9330127018922191873, 0.9330127018922192983 ) ) 
 REPRESENTATION_ITEM ( '' )  );
#7187 = DIRECTION ( 'NONE',  ( 0.000000000000000000, 0.000000000000000000, -1.000000000000000000 ) ) ;
#7188 = CARTESIAN_POINT ( 'NONE',  ( -2.649999999999885780, 30.00000000000000000, -2.500000000000000000 ) ) ;
#7189 = VECTOR ( 'NONE', #2894, 1000.000000000000000 ) ;
#7191 = EDGE_CURVE ( 'NONE', #8667, #4515, #8769, .T. ) ;
#7190 = LINE ( 'NONE', #4486, #4238 ) ;
#7192 = CARTESIAN_POINT ( 'NONE',  ( -2.474873734152916338, 27.52512626584707789, 15.37500000000000355 ) ) ;
#7193 = CARTESIAN_POINT ( 'NONE',  ( -25.98076211353311393, 49.49999999999986500, -7.000000000000074607 ) ) ;
#7194 = ORIENTED_EDGE ( 'NONE', *, *, #2585, .F. ) ;
#7195 = FACE_OUTER_BOUND ( 'NONE', #6391, .T. ) ;
#7196 = CIRCLE ( 'NONE', #7551, 3.499999999999999556 ) ;
#7197 = CARTESIAN_POINT ( 'NONE',  ( -1.515916693951006478, 26.52740819067394895, 15.20093341526694353 ) ) ;
#7198 = CARTESIAN_POINT ( 'NONE',  ( 3.500000000000007994, 29.93383077435482420, 15.59155841526693997 ) ) ;
#7199 = VECTOR ( 'NONE', #6406, 1000.000000000000000 ) ;
#7200 = CARTESIAN_POINT ( 'NONE',  ( 22.03595509826854126, 19.06622527062933870, 12.00579112326941988 ) ) ;
#7201 = FACE_BOUND ( 'NONE', #4351, .T. ) ;
#7202 = CARTESIAN_POINT ( 'NONE',  ( -26.51666049839535333, 51.39373926088290290, -3.000000000000132339 ) ) ;
#7203 = CARTESIAN_POINT ( 'NONE',  ( -26.79131905728310059, 51.76041666571061484, -3.596074190997381237 ) ) ;
#7204 = CARTESIAN_POINT ( 'NONE',  ( 3.200000000000001510, 2.686816014504541439, -2.346298152288397443 ) ) ;
#7205 = CARTESIAN_POINT ( 'NONE',  ( -27.98076211353308551, 55.44999999999986073, -5.000000000000103029 ) ) ;
#7206 = VECTOR ( 'NONE', #4301, 999.9999999999998863 ) ;
#7207 = ORIENTED_EDGE ( 'NONE', *, *, #236, .F. ) ;
#7208 = DIRECTION ( 'NONE',  ( -1.000000000000000000, -0.000000000000000000, -0.000000000000000000 ) ) ;
#7209 = APPLICATION_CONTEXT ( 'automotive_design' ) ;
#7210 = PRODUCT_CONTEXT ( 'NONE', #4382, 'mechanical' ) ;
#7211 = EDGE_LOOP ( 'NONE', ( #7382, #751, #3951, #330 ) ) ;
#7212 = FACE_OUTER_BOUND ( 'NONE', #3023, .T. ) ;
#7213 = AXIS2_PLACEMENT_3D ( 'NONE', #5360, #8741, #10580 ) ;
#7214 = CARTESIAN_POINT ( 'NONE',  ( -27.60187600103308370, 50.06874999904395196, -5.000000000000103029 ) ) ;
#7215 = CARTESIAN_POINT ( 'NONE',  ( 20.70533613433985920, 18.20808090964021986, 11.00732503135576401 ) ) ;
#7216 = VERTEX_POINT ( 'NONE', #8828 ) ;
#7217 = CARTESIAN_POINT ( 'NONE',  ( 34.90196196521935690, 2.620161469061431436, 3.662783066803843468 ) ) ;
#7218 = VERTEX_POINT ( 'NONE', #1994 ) ;
#7219 = CARTESIAN_POINT ( 'NONE',  ( -4.379688272585405606, 36.08837668307224789, 2.500000000000000000 ) ) ;
#7220 = ORIENTED_EDGE ( 'NONE', *, *, #5469, .T. ) ;
#7221 = CARTESIAN_POINT ( 'NONE',  ( -1.035533905932742638, 32.50000000000000000, 14.98437500000000711 ) ) ;
#7222 = ORIENTED_EDGE ( 'NONE', *, *, #9123, .F. ) ;
#7224 = CARTESIAN_POINT ( 'NONE',  ( 22.05490153526506703, 17.93057544254518376, 10.95195840513859231 ) ) ;
#7223 = AXIS2_PLACEMENT_3D ( 'NONE', #8793, #290, #6234 ) ;
#7225 = PRODUCT_DEFINITION_FORMATION_WITH_SPECIFIED_SOURCE ( 'ANY', '', #5290, .NOT_KNOWN. ) ;
#7226 = ADVANCED_FACE ( 'NONE', ( #3770 ), #1887, .T. ) ;
#7227 = DIRECTION ( 'NONE',  ( 1.000000000000000000, 6.098637220230963674E-17, 1.156482317317871478E-16 ) ) ;
#7228 = EDGE_CURVE ( 'NONE', #670, #2953, #2030, .T. ) ;
#7229 = CARTESIAN_POINT ( 'NONE',  ( 19.98916778955327800, 17.57501987461890991, 13.00425721518307576 ) ) ;
#7230 = VECTOR ( 'NONE', #8679, 1000.000000000000000 ) ;
#7231 = AXIS2_PLACEMENT_3D ( 'NONE', #9784, #5725, #7330 ) ;
#7232 = DIRECTION ( 'NONE',  ( -1.000000000000000000, -6.098637220230963674E-17, -1.156482317317871478E-16 ) ) ;
#7233 = PLANE ( 'NONE',  #3690 ) ;
#7234 = ORIENTED_EDGE ( 'NONE', *, *, #6494, .T. ) ;
#7235 = ORIENTED_EDGE ( 'NONE', *, *, #5390, .T. ) ;
#7236 = CARTESIAN_POINT ( 'NONE',  ( 17.41267794807257374, 17.53706952023173216, 13.10128505860060066 ) ) ;
#7237 = CIRCLE ( 'NONE', #5127, 4.499999999999999112 ) ;
#7238 = CARTESIAN_POINT ( 'NONE',  ( 4.000000000000000000, 0.000000000000000000, 0.000000000000000000 ) ) ;
#7239 = CARTESIAN_POINT ( 'NONE',  ( -31.74999999999995737, 0.000000000000000000, 0.000000000000000000 ) ) ;
#7240 = CIRCLE ( 'NONE', #9554, 3.299999999999999822 ) ;
#7241 = CARTESIAN_POINT ( 'NONE',  ( 0.2182762428107514474, 1.693953258775869442, 3.499999999999999556 ) ) ;
#7242 = CARTESIAN_POINT ( 'NONE',  ( -25.84741345379021737, 56.99999999999889155, -7.000000000000078160 ) ) ;
#7243 = CARTESIAN_POINT ( 'NONE',  ( 2.887392608830845031, -2.020725942164465661, -3.499999999999999556 ) ) ;
#7244 = CARTESIAN_POINT ( 'NONE',  ( -3.500000000000002665, 29.72450764647708255, 16.48359592357600434 ) ) ;
#7245 = PLANE ( 'NONE',  #3657 ) ;
#7246 = EDGE_LOOP ( 'NONE', ( #3674, #2395, #7207, #4173, #9211, #6939, #7968, #667 ) ) ;
#7247 = DIRECTION ( 'NONE',  ( -1.156482317317871725E-16, 0.000000000000000000, 1.000000000000000000 ) ) ;
#7248 = TOROIDAL_SURFACE ( 'NONE', #8676, 2.200000000000001066, 0.2000000000000000111 ) ;
#7249 = CIRCLE ( 'NONE', #152, 3.249999999999999556 ) ;
#7250 = CARTESIAN_POINT ( 'NONE',  ( 2.500000000000009770, 29.93383077435482420, 16.84155841526694175 ) ) ;
#7251 = CARTESIAN_POINT ( 'NONE',  ( -25.98076211353311393, 49.49999999999986500, -5.000000000000103029 ) ) ;
#7252 =( BOUNDED_CURVE ( )  B_SPLINE_CURVE ( 3, ( #2611, #2548, #5828, #3441 ),
 .UNSPECIFIED., .F., .F. ) 
 B_SPLINE_CURVE_WITH_KNOTS ( ( 4, 4 ),
 ( 3.469446951953614189E-18, 0.001563228649568143037 ),
 .UNSPECIFIED. ) 
 CURVE ( )  GEOMETRIC_REPRESENTATION_ITEM ( )  RATIONAL_B_SPLINE_CURVE ( ( 1.000000000000000000, 0.3333333333333327597, 0.3333333333333334814, 1.000000000000000666 ) ) 
 REPRESENTATION_ITEM ( '' )  );
#7253 = CARTESIAN_POINT ( 'NONE',  ( 19.86292016999849608, 19.38279280778333202, 11.97810781016083403 ) ) ;
#7254 = CARTESIAN_POINT ( 'NONE',  ( -25.44486372867087809, 53.46876073720499534, -3.000000000000132339 ) ) ;
#7255 = DIRECTION ( 'NONE',  ( 0.000000000000000000, 0.000000000000000000, -1.000000000000000000 ) ) ;
#7256 = CARTESIAN_POINT ( 'NONE',  ( -25.98076211353311393, 53.56874999904394485, -6.871901078670400231 ) ) ;
#7257 = ADVANCED_FACE ( 'NONE', ( #9487, #5277 ), #2206, .T. ) ;
#7258 = CARTESIAN_POINT ( 'NONE',  ( 4.000000000000001776, 2.694222958124178486E-16, 2.200000000000001066 ) ) ;
#7259 = CARTESIAN_POINT ( 'NONE',  ( -1.274258131565027874, -3.883108878240886241, -3.220599429844051009 ) ) ;
#7260 = ORIENTED_EDGE ( 'NONE', *, *, #8339, .F. ) ;
#7261 = DIRECTION ( 'NONE',  ( 0.8191520442889902442, 1.003171929053522651E-16, -0.5735764363510482688 ) ) ;
#7262 = DIRECTION ( 'NONE',  ( -0.000000000000000000, 0.000000000000000000, 1.000000000000000000 ) ) ;
#7263 = CONTEXT_DEPENDENT_SHAPE_REPRESENTATION ( #5713, #6873 ) ;
#7264 = ORIENTED_EDGE ( 'NONE', *, *, #7627, .T. ) ;
#7265 = DIRECTION ( 'NONE',  ( -0.000000000000000000, 0.000000000000000000, 1.000000000000000000 ) ) ;
#7266 = CARTESIAN_POINT ( 'NONE',  ( -27.60187600103308725, 50.82708333237729192, -4.064049460664955760 ) ) ;
#7267 = CARTESIAN_POINT ( 'NONE',  ( 22.41005638895160601, 19.39388128063383476, 11.00732503135576401 ) ) ;
#7268 = ORIENTED_EDGE ( 'NONE', *, *, #7170, .T. ) ;
#7269 = DIRECTION ( 'NONE',  ( 0.000000000000000000, 1.224646799147353207E-16, 1.000000000000000000 ) ) ;
#7270 = ORIENTED_EDGE ( 'NONE', *, *, #10301, .T. ) ;
#7271 = CARTESIAN_POINT ( 'NONE',  ( -2.963055325167751164, 29.53063538693776735, 16.49922112211940117 ) ) ;
#7272 = EDGE_LOOP ( 'NONE', ( #5145, #7637, #8678, #1027, #95, #8199 ) ) ;
#7273 = CARTESIAN_POINT ( 'NONE',  ( 25.00000000000000000, 2.789133085058098087E-16, -2.055000000000000160 ) ) ;
#7274 =( NAMED_UNIT ( * ) SI_UNIT ( $, .STERADIAN. ) SOLID_ANGLE_UNIT ( ) );
#7275 = ORIENTED_EDGE ( 'NONE', *, *, #8526, .F. ) ;
#7276 = PRODUCT_RELATED_PRODUCT_CATEGORY ( 'part', '', ( #3417 ) ) ;
#7277 = CARTESIAN_POINT ( 'NONE',  ( 16.86040243112223180, 16.67515725582037689, 11.08237315523004973 ) ) ;
#7278 = CARTESIAN_POINT ( 'NONE',  ( 29.50000000000000711, 5.000000000000001776, 5.500000000000000000 ) ) ;
#7279 = CARTESIAN_POINT ( 'NONE',  ( 22.67082259973814828, 19.44041185113230341, 13.00425721518326938 ) ) ;
#7280 = CARTESIAN_POINT ( 'NONE',  ( -23.98076211353314235, 50.75416666475469185, -3.845299461620867554 ) ) ;
#7281 = DIRECTION ( 'NONE',  ( 6.098637220230963674E-17, -1.000000000000000000, 0.000000000000000000 ) ) ;
#7282 = PLANE ( 'NONE',  #7955 ) ;
#7283 = ORIENTED_EDGE ( 'NONE', *, *, #6203, .T. ) ;
#7284 = ORIENTED_EDGE ( 'NONE', *, *, #4672, .T. ) ;
#7285 = EDGE_CURVE ( 'NONE', #8126, #3122, #6476, .T. ) ;
#7286 = CARTESIAN_POINT ( 'NONE',  ( 22.44007493706583745, 19.34731747087121434, 12.00579112326928133 ) ) ;
#7287 = EDGE_CURVE ( 'NONE', #7090, #1840, #1133, .T. ) ;
#7288 = AXIS2_PLACEMENT_3D ( 'NONE', #6519, #633, #8356 ) ;
#7289 = CARTESIAN_POINT ( 'NONE',  ( 0.000000000000000000, 0.000000000000000000, 3.499999999999999556 ) ) ;
#7290 = CARTESIAN_POINT ( 'NONE',  ( 6.015568632492056977, 34.47916666666665009, 0.000000000000000000 ) ) ;
#7291 = CARTESIAN_POINT ( 'NONE',  ( 4.000000000000000000, 0.000000000000000000, 0.000000000000000000 ) ) ;
#7292 = CARTESIAN_POINT ( 'NONE',  ( 3.500000000000003997, 30.06616922564517580, 14.84594158473306713 ) ) ;
#7293 = DIRECTION ( 'NONE',  ( -0.000000000000000000, -0.000000000000000000, -1.000000000000000000 ) ) ;
#7294 = UNCERTAINTY_MEASURE_WITH_UNIT (LENGTH_MEASURE( 1.000000000000000082E-05 ), #5535, 'distance_accuracy_value', 'NONE');
#7295 = DIRECTION ( 'NONE',  ( -6.098637220230964906E-17, 1.000000000000000000, 0.000000000000000000 ) ) ;
#7296 = CARTESIAN_POINT ( 'NONE',  ( 29.49999999999999289, 5.000000000000002665, -2.500000000000000000 ) ) ;
#7297 = ADVANCED_FACE ( 'NONE', ( #7370 ), #7422, .F. ) ;
#7298 = ORIENTED_EDGE ( 'NONE', *, *, #5536, .T. ) ;
#7299 = AXIS2_PLACEMENT_3D ( 'NONE', #3656, #6933, #6256 ) ;
#7300 = CARTESIAN_POINT ( 'NONE',  ( 2.500000000000009770, 29.93383077435482420, 15.59155841526693997 ) ) ;
#7301 = CARTESIAN_POINT ( 'NONE',  ( 3.200000000000000178, 0.000000000000000000, 0.000000000000000000 ) ) ;
#7302 = CARTESIAN_POINT ( 'NONE',  ( 24.49999999999999289, -8.499999999999984013, 10.00000000000001243 ) ) ;
#7303 = CARTESIAN_POINT ( 'NONE',  ( -2.385244779468109755E-15, 32.50000000000000711, 13.65625000000000355 ) ) ;
#7304 = ADVANCED_FACE ( 'NONE', ( #3048 ), #4825, .T. ) ;
#7305 = DIRECTION ( 'NONE',  ( 0.8660254037844398178, 0.4999999999999978351, 0.000000000000000000 ) ) ;
#7306 = CARTESIAN_POINT ( 'NONE',  ( -25.17020516978313083, 50.53541666571062052, -6.403925809002825709 ) ) ;
#7307 = LINE ( 'NONE', #7471, #8911 ) ;
#7308 = CARTESIAN_POINT ( 'NONE',  ( -26.98076211353309972, 55.33333333333320070, -6.732050807568954909 ) ) ;
#7309 = VERTEX_POINT ( 'NONE', #6423 ) ;
#7310 = CARTESIAN_POINT ( 'NONE',  ( 2.500000000000000000, -2.629050547790028551E-15, -2.041999999999999815 ) ) ;
#7311 = VECTOR ( 'NONE', #9376, 1000.000000000000000 ) ;
#7312 = CARTESIAN_POINT ( 'NONE',  ( 25.98076211353324183, 54.99999999999984368, -2.500000000000000000 ) ) ;
#7313 = CONTEXT_DEPENDENT_SHAPE_REPRESENTATION ( #1069, #6970 ) ;
#7314 = EDGE_CURVE ( 'NONE', #9083, #7830, #2928, .T. ) ;
#7315 = CARTESIAN_POINT ( 'NONE',  ( -24.35964822603314772, 50.53541666571060631, -4.064049460664953983 ) ) ;
#7316 = CARTESIAN_POINT ( 'NONE',  ( -27.60187600103308370, 53.56874999904395196, -5.000000000000103029 ) ) ;
#7317 = AXIS2_PLACEMENT_3D ( 'NONE', #4508, #9389, #10390 ) ;
#7318 = CARTESIAN_POINT ( 'NONE',  ( 23.13231036272843966, 20.08340223762181154, 12.00579112326941988 ) ) ;
#7319 = CARTESIAN_POINT ( 'NONE',  ( -26.79131905728310059, 54.38541666571061484, -3.596074190997381237 ) ) ;
#7320 = VERTEX_POINT ( 'NONE', #9980 ) ;
#7321 = CARTESIAN_POINT ( 'NONE',  ( 34.94281041931229481, 2.000000000000001332, 5.102623512424888652 ) ) ;
#7322 = ADVANCED_BREP_SHAPE_REPRESENTATION ( '', ( #5271, #308 ), #3340 ) ;
#7323 = ORIENTED_EDGE ( 'NONE', *, *, #8938, .T. ) ;
#7324 = CARTESIAN_POINT ( 'NONE',  ( -3.861362476283256129, -2.629030857716004199, -3.671615880910374941 ) ) ;
#7325 = VERTEX_POINT ( 'NONE', #3927 ) ;
#7326 = CARTESIAN_POINT ( 'NONE',  ( 1.035533905932737975, 32.50000000000000711, 16.07812500000000355 ) ) ;
#7327 = ORIENTED_EDGE ( 'NONE', *, *, #7170, .F. ) ;
#7328 = CARTESIAN_POINT ( 'NONE',  ( 20.49609864019753402, 16.84626017008312360, 10.95195840513859231 ) ) ;
#7329 =( LENGTH_UNIT ( ) NAMED_UNIT ( * ) SI_UNIT ( .MILLI., .METRE. ) );
#7330 = DIRECTION ( 'NONE',  ( 0.000000000000000000, 0.000000000000000000, -1.000000000000000000 ) ) ;
#7331 = CARTESIAN_POINT ( 'NONE',  ( 16.50280774463635680, 17.03272616129868666, 12.11810441208646338 ) ) ;
#7332 = CARTESIAN_POINT ( 'NONE',  ( -25.98076211353311393, 51.33749999808802755, -2.690598923241634743 ) ) ;
#7333 = CARTESIAN_POINT ( 'NONE',  ( 34.99999999999999289, -3.999999999999993339, 10.00000000000000533 ) ) ;
#7334 = CARTESIAN_POINT ( 'NONE',  ( 2.649999999999991029, 30.00000000000000000, 2.500000000000000000 ) ) ;
#7335 = EDGE_CURVE ( 'NONE', #8932, #7431, #4269, .T. ) ;
#7336 = ORIENTED_EDGE ( 'NONE', *, *, #5298, .T. ) ;
#7337 = ORIENTED_EDGE ( 'NONE', *, *, #7967, .F. ) ;
#7338 = CARTESIAN_POINT ( 'NONE',  ( 21.25655365073496839, 18.52406763439849513, 12.00579112326941988 ) ) ;
#7339 = VECTOR ( 'NONE', #5813, 1000.000000000000000 ) ;
#7340 = DIRECTION ( 'NONE',  ( 0.000000000000000000, 0.000000000000000000, -1.000000000000000000 ) ) ;
#7341 = DIRECTION ( 'NONE',  ( 0.000000000000000000, -1.000000000000000000, 0.000000000000000000 ) ) ;
#7342 = DIRECTION ( 'NONE',  ( -1.000000000000000000, -0.000000000000000000, -0.000000000000000000 ) ) ;
#7343 = CIRCLE ( 'NONE', #9843, 2.700000000000001066 ) ;
#7344 = ADVANCED_FACE ( 'NONE', ( #5706 ), #1319, .F. ) ;
#7345 = CARTESIAN_POINT ( 'NONE',  ( -2.521662442312484931, 32.42808502599334730, 15.31469158473306713 ) ) ;
#7346 = DIRECTION ( 'NONE',  ( 0.000000000000000000, 1.000000000000000000, 0.000000000000000000 ) ) ;
#7347 = VECTOR ( 'NONE', #6765, 1000.000000000000000 ) ;
#7348 = VERTEX_POINT ( 'NONE', #3097 ) ;
#7349 = CARTESIAN_POINT ( 'NONE',  ( -26.51666049839534622, 55.50623925897107114, -3.000000000000131006 ) ) ;
#7350 = ADVANCED_FACE ( 'NONE', ( #4775 ), #1430, .T. ) ;
#7351 = ORIENTED_EDGE ( 'NONE', *, *, #5043, .T. ) ;
#7352 = CARTESIAN_POINT ( 'NONE',  ( -2.428085025993355295, 32.52166244231248271, 14.81030841526694175 ) ) ;
#7353 = CIRCLE ( 'NONE', #6814, 4.000000000000000000 ) ;
#7354 = DIRECTION ( 'NONE',  ( -1.000000000000000000, -6.098637220230963674E-17, 0.000000000000000000 ) ) ;
#7355 = DIRECTION ( 'NONE',  ( 0.000000000000000000, -0.5000000000000012212, -0.8660254037844380415 ) ) ;
#7356 = CIRCLE ( 'NONE', #8784, 3.499999999999997780 ) ;
#7357 = CARTESIAN_POINT ( 'NONE',  ( 30.75045812061784289, 53.49999999999983658, 14.50000000000000000 ) ) ;
#7358 = ADVANCED_FACE ( 'NONE', ( #3878 ), #4035, .T. ) ;
#7359 = CARTESIAN_POINT ( 'NONE',  ( 34.93845944406324122, 2.080102445711407011, 4.707808283735069210 ) ) ;
#7360 = CARTESIAN_POINT ( 'NONE',  ( -27.60187600103308014, 50.12708333237727487, -4.064049460664955760 ) ) ;
#7361 = ADVANCED_FACE ( 'NONE', ( #2158 ), #2315, .F. ) ;
#7362 = LINE ( 'NONE', #525, #4310 ) ;
#7363 = CARTESIAN_POINT ( 'NONE',  ( -25.98076211353311393, 55.27499999999985647, -7.000000000000072831 ) ) ;
#7364 = AXIS2_PLACEMENT_3D ( 'NONE', #7946, #1220, #2845 ) ;
#7365 = ORIENTED_EDGE ( 'NONE', *, *, #9983, .T. ) ;
#7366 =( BOUNDED_CURVE ( )  B_SPLINE_CURVE ( 2, ( #4591, #4532, #9633, #511, #10684, #3694, #2025, #5418, #3747 ),
 .UNSPECIFIED., .F., .F. ) 
 B_SPLINE_CURVE_WITH_KNOTS ( ( 3, 2, 2, 2, 3 ),
 ( 0.3611111111111111605, 0.3703703703703703498, 0.3888888888888888951, 0.4074074074074073848, 0.4166666666666666852 ),
 .UNSPECIFIED. ) 
 CURVE ( )  GEOMETRIC_REPRESENTATION_ITEM ( )  RATIONAL_B_SPLINE_CURVE ( ( 0.9330127018922194093, 0.9330127018922197424, 1.000000000000000000, 0.8660254037844387076, 1.000000000000000000, 0.8660254037844387076, 1.000000000000000000, 0.9330127018922191873, 0.9330127018922194093 ) ) 
 REPRESENTATION_ITEM ( '' )  );
#7367 = AXIS2_PLACEMENT_3D ( 'NONE', #5407, #7965, #9623 ) ;
#7368 = CARTESIAN_POINT ( 'NONE',  ( -21.21106610644865498, 13.49999999999941913, -2.500000000000000000 ) ) ;
#7369 = AXIS2_PLACEMENT_3D ( 'NONE', #8870, #8811, #6453 ) ;
#7370 = FACE_OUTER_BOUND ( 'NONE', #9261, .T. ) ;
#7371 = CARTESIAN_POINT ( 'NONE',  ( -26.79131905728310059, 50.36041666571060915, -3.596074190997381237 ) ) ;
#7372 = AXIS2_PLACEMENT_3D ( 'NONE', #9909, #10681, #3954 ) ;
#7373 = CARTESIAN_POINT ( 'NONE',  ( -27.60187600103308370, 52.16874999904395338, -5.000000000000103029 ) ) ;
#7374 = AXIS2_PLACEMENT_3D ( 'NONE', #2587, #5968, #1579 ) ;
#7375 = CARTESIAN_POINT ( 'NONE',  ( 19.77604874367146692, 21.01153129092389094, 12.00579112326941988 ) ) ;
#7376 = CARTESIAN_POINT ( 'NONE',  ( -25.17020516978313083, 54.50208333237728198, -3.596074190997380349 ) ) ;
#7377 = ORIENTED_EDGE ( 'NONE', *, *, #9972, .T. ) ;
#7378 = CARTESIAN_POINT ( 'NONE',  ( 3.199999999999992628, -2.859595677584409135, -2.047034997319491900 ) ) ;
#7379 = EDGE_LOOP ( 'NONE', ( #986, #1352, #4750, #2903, #7336, #8392 ) ) ;
#7380 = VERTEX_POINT ( 'NONE', #1536 ) ;
#7381 = CARTESIAN_POINT ( 'NONE',  ( 4.200000000000001954, 0.000000000000000000, 0.000000000000000000 ) ) ;
#7382 = ORIENTED_EDGE ( 'NONE', *, *, #6325, .F. ) ;
#7383 = CARTESIAN_POINT ( 'NONE',  ( 29.50000000000000711, -3.999999999999989786, 9.999999999999998224 ) ) ;
#7384 = VECTOR ( 'NONE', #2194, 1000.000000000000000 ) ;
#7385 = VERTEX_POINT ( 'NONE', #641 ) ;
#7386 = CARTESIAN_POINT ( 'NONE',  ( 19.89794927727885110, 21.35687623891577758, 11.00732503135556861 ) ) ;
#7387 = CARTESIAN_POINT ( 'NONE',  ( 0.6640947660595348800, -4.471078309994175548, -3.602146406945708090 ) ) ;
#7388 = CARTESIAN_POINT ( 'NONE',  ( 19.36223501247343393, 16.11237126175916501, 11.95718771041564210 ) ) ;
#7389 = CARTESIAN_POINT ( 'NONE',  ( -27.98076211353308551, 51.86249999808803324, -5.000000000000103029 ) ) ;
#7390 = CARTESIAN_POINT ( 'NONE',  ( 34.94170751511534689, 2.019541143081656109, -5.105981766738329597 ) ) ;
#7391 = CARTESIAN_POINT ( 'NONE',  ( -2.500000000000000888, 0.000000000000000000, -4.974599999999998801 ) ) ;
#7392 = ORIENTED_EDGE ( 'NONE', *, *, #9182, .F. ) ;
#7393 = STYLED_ITEM ( 'NONE', ( #2224 ), #10767 ) ;
#7394 = CARTESIAN_POINT ( 'NONE',  ( 1.383578242660662871, 26.47259180932604039, 16.60718341526694175 ) ) ;
#7395 = ORIENTED_EDGE ( 'NONE', *, *, #1832, .F. ) ;
#7396 = CARTESIAN_POINT ( 'NONE',  ( 22.69616945897178084, 19.53356342368596898, 12.00579112326941988 ) ) ;
#7397 = CARTESIAN_POINT ( 'NONE',  ( -23.98076211353314235, 52.35833333333319217, -6.154700538379337615 ) ) ;
#7398 = CIRCLE ( 'NONE', #8649, 1.650000000000000355 ) ;
#7399 = CIRCLE ( 'NONE', #6505, 2.000000000000000000 ) ;
#7400 = CARTESIAN_POINT ( 'NONE',  ( 34.99999999999987210, 2.000000000000002220, -12.50000000000000000 ) ) ;
#7401 = CARTESIAN_POINT ( 'NONE',  ( -2.000000000000006661, 3.464101615137750834, 0.000000000000000000 ) ) ;
#7402 = CARTESIAN_POINT ( 'NONE',  ( 0.06616922564517879746, 26.50000000000000000, 14.53344158473306535 ) ) ;
#7403 = CARTESIAN_POINT ( 'NONE',  ( 5.000000000000002665, 3.306546357697854226E-16, 2.700000000000001066 ) ) ;
#7404 = ORIENTED_EDGE ( 'NONE', *, *, #4841, .T. ) ;
#7405 = FACE_OUTER_BOUND ( 'NONE', #6567, .T. ) ;
#7406 = ORIENTED_EDGE ( 'NONE', *, *, #3231, .T. ) ;
#7407 = CIRCLE ( 'NONE', #841, 2.649999999999991029 ) ;
#7408 = CARTESIAN_POINT ( 'NONE',  ( -3.527408190673961386, 28.61642175733934224, 15.04468341526694175 ) ) ;
#7409 = CARTESIAN_POINT ( 'NONE',  ( 3.319999999999999840, 0.000000000000000000, 0.000000000000000000 ) ) ;
#7410 = COLOUR_RGB ( '', 0.09019608, 0.27058824, 0.51372549) ;
#7411 = CARTESIAN_POINT ( 'NONE',  ( 17.59356678224322934, 17.35619608210146581, 12.08212522340233264 ) ) ;
#7412 = APPLICATION_CONTEXT ( 'automotive_design' ) ;
#7413 = DIRECTION ( 'NONE',  ( 1.000000000000000000, 0.000000000000000000, 0.000000000000000000 ) ) ;
#7414 = CARTESIAN_POINT ( 'NONE',  ( -25.98076211353311393, 52.82499999999986784, -3.000000000000132339 ) ) ;
#7415 = CARTESIAN_POINT ( 'NONE',  ( -24.35964822603314772, 50.47708333237728340, -5.935950539335252074 ) ) ;
#7416 = CARTESIAN_POINT ( 'NONE',  ( 2.887392608830354757, -4.041451884327390331, 2.328390191177121598E-14 ) ) ;
#7417 = AXIS2_PLACEMENT_3D ( 'NONE', #4474, #9680, #1968 ) ;
#7418 = CARTESIAN_POINT ( 'NONE',  ( 4.197478902586992966, -0.8524102783748346290, -3.505063281295504041 ) ) ;
#7419 = VERTEX_POINT ( 'NONE', #10812 ) ;
#7420 =( GEOMETRIC_REPRESENTATION_CONTEXT ( 3 ) GLOBAL_UNCERTAINTY_ASSIGNED_CONTEXT ( ( #9859 ) ) GLOBAL_UNIT_ASSIGNED_CONTEXT ( ( #7500, #1303, #4698 ) ) REPRESENTATION_CONTEXT ( 'NONE', 'WORKASPACE' ) );
#7421 = CARTESIAN_POINT ( 'NONE',  ( 3.903127820947815962E-15, 26.49999999999999289, 14.28125000000000355 ) ) ;
#7422 = CYLINDRICAL_SURFACE ( 'NONE', #68, 1.000000000000972333 ) ;
#7423 = EDGE_CURVE ( 'NONE', #6424, #10663, #5579, .T. ) ;
#7424 = ADVANCED_FACE ( 'NONE', ( #10604 ), #2373, .F. ) ;
#7425 = CARTESIAN_POINT ( 'NONE',  ( -24.98076211353193798, 57.99999999999910472, -3.267949192431741423 ) ) ;
#7426 = CARTESIAN_POINT ( 'NONE',  ( -24.35964822603314417, 52.51874999904394770, -5.000000000000103029 ) ) ;
#7427 = CARTESIAN_POINT ( 'NONE',  ( 22.69616945897178084, 19.53356342368596898, 12.00579112326941988 ) ) ;
#7428 = CARTESIAN_POINT ( 'NONE',  ( -24.35964822603314772, 54.67708333237728624, -5.935950539335252074 ) ) ;
#7429 = EDGE_LOOP ( 'NONE', ( #6457, #1619, #6174, #7268 ) ) ;
#7430 = DIRECTION ( 'NONE',  ( -0.000000000000000000, 1.000000000000000000, 1.224646799147353207E-16 ) ) ;
#7431 = VERTEX_POINT ( 'NONE', #6378 ) ;
#7432 = ORIENTED_EDGE ( 'NONE', *, *, #8873, .T. ) ;
#7433 = DIRECTION ( 'NONE',  ( 1.000000000000000000, 0.000000000000000000, 0.000000000000000000 ) ) ;
#7434 = VERTEX_POINT ( 'NONE', #2537 ) ;
#7435 = ADVANCED_FACE ( 'NONE', ( #9251 ), #4205, .F. ) ;
#7436 = CARTESIAN_POINT ( 'NONE',  ( 1.035533905932743970, 27.49999999999999289, 15.60937500000000711 ) ) ;
#7437 = DIRECTION ( 'NONE',  ( 1.000000000000000000, 0.000000000000000000, 0.000000000000000000 ) ) ;
#7438 = ORIENTED_EDGE ( 'NONE', *, *, #4225, .F. ) ;
#7439 = CARTESIAN_POINT ( 'NONE',  ( 19.01572293645009637, 17.10672457250295508, 11.01141524516921422 ) ) ;
#7440 = FILL_AREA_STYLE_COLOUR ( '', #2453 ) ;
#7441 = CARTESIAN_POINT ( 'NONE',  ( -4.000000000000000000, 0.3987449864459974846, -0.01220643443059782861 ) ) ;
#7442 = DIRECTION ( 'NONE',  ( 4.312387734422005941E-17, -0.7071067811865500152, -0.7071067811865451302 ) ) ;
#7443 = EDGE_CURVE ( 'NONE', #10877, #8683, #7186, .T. ) ;
#7444 = CARTESIAN_POINT ( 'NONE',  ( 23.26157621925297647, 18.63507786824203549, 12.94889058896600353 ) ) ;
#7445 = CARTESIAN_POINT ( 'NONE',  ( -27.98076211353308551, 51.10416666475470748, -6.154700538379338504 ) ) ;
#7446 = FACE_OUTER_BOUND ( 'NONE', #5112, .T. ) ;
#7447 = LINE ( 'NONE', #10890, #5118 ) ;
#7448 = PRODUCT_DEFINITION_CONTEXT ( 'detailed design', #10477, 'design' ) ;
#7449 = B_SPLINE_CURVE_WITH_KNOTS ( 'NONE', 3,
 ( #245, #142, #4438, #1867, #4376, #4318, #7706, #5209 ),
 .UNSPECIFIED., .F., .F.,
 ( 4, 2, 2, 4 ),
 ( 2.465131517071610173E-07, 0.001183067374689837636, 0.001774477805458902699, 0.002365888236227967761 ),
 .UNSPECIFIED. ) ;
#7450 = ORIENTED_EDGE ( 'NONE', *, *, #8301, .F. ) ;
#7451 = CARTESIAN_POINT ( 'NONE',  ( 0.06616922564517314920, 33.50000000000000000, 14.65405841526694353 ) ) ;
#7452 = ORIENTED_EDGE ( 'NONE', *, *, #1240, .F. ) ;
#7453 = CARTESIAN_POINT ( 'NONE',  ( 22.06757164964230711, 19.02077357123424406, 13.00425721518307576 ) ) ;
#7454 = EDGE_CURVE ( 'NONE', #8327, #670, #84, .T. ) ;
#7455 = LINE ( 'NONE', #8131, #1510 ) ;
#7456 = PLANE ( 'NONE',  #7465 ) ;
#7457 = CARTESIAN_POINT ( 'NONE',  ( -25.98076211353311393, 49.49999999999986500, -7.000000000000074607 ) ) ;
#7458 = CARTESIAN_POINT ( 'NONE',  ( 1.515916693951011140, 26.52740819067395250, 14.61156658473306713 ) ) ;
#7459 = CARTESIAN_POINT ( 'NONE',  ( 15.83212018001054133, 17.70341372592255524, 11.17880707182957778 ) ) ;
#7460 = CARTESIAN_POINT ( 'NONE',  ( -30.75045812061784289, 13.49999999999941913, -2.500000000000000000 ) ) ;
#7461 = CARTESIAN_POINT ( 'NONE',  ( 2.887392608830347207, 2.020725942163738686, 3.499999999999999556 ) ) ;
#7462 = VERTEX_POINT ( 'NONE', #9369 ) ;
#7463 = EDGE_LOOP ( 'NONE', ( #4306, #8840, #8050 ) ) ;
#7464 = CARTESIAN_POINT ( 'NONE',  ( -27.98076211353308551, 51.94999999999986784, -5.000000000000103029 ) ) ;
#7465 = AXIS2_PLACEMENT_3D ( 'NONE', #5081, #4854, #10899 ) ;
#7466 = DIRECTION ( 'NONE',  ( -1.000000000000000000, -6.098637220230963674E-17, -1.156482317317871725E-16 ) ) ;
#7467 = CARTESIAN_POINT ( 'NONE',  ( -23.98076211353314235, 52.21249999808803466, -5.000000000000103029 ) ) ;
#7468 = CARTESIAN_POINT ( 'NONE',  ( -27.78269984933782411, 56.11211482050296695, -4.132232521764788835 ) ) ;
#7469 = CARTESIAN_POINT ( 'NONE',  ( 25.49999999999999645, -3.999999999999983569, 8.350000000000010303 ) ) ;
#7470 = CARTESIAN_POINT ( 'NONE',  ( -24.35964822603314772, 54.85208333237728340, -5.935950539335252074 ) ) ;
#7471 = CARTESIAN_POINT ( 'NONE',  ( -30.31088913245546124, 17.49999999999980815, 2.500000000000000000 ) ) ;
#7472 = DIRECTION ( 'NONE',  ( 0.000000000000000000, 0.000000000000000000, -1.000000000000000000 ) ) ;
#7473 = AXIS2_PLACEMENT_3D ( 'NONE', #4185, #7342, #9175 ) ;
#7474 = VERTEX_POINT ( 'NONE', #2601 ) ;
#7475 = EDGE_CURVE ( 'NONE', #3122, #3024, #1767, .T. ) ;
#7476 = CARTESIAN_POINT ( 'NONE',  ( -2.500000000000007550, 31.03553390593274486, 13.89062500000000355 ) ) ;
#7477 = ADVANCED_FACE ( 'NONE', ( #10150 ), #800, .T. ) ;
#7478 = FACE_BOUND ( 'NONE', #537, .T. ) ;
#7479 = B_SPLINE_CURVE_WITH_KNOTS ( 'NONE', 3,
 ( #7461, #1576, #4975, #8348, #3300, #6681 ),
 .UNSPECIFIED., .F., .F.,
 ( 4, 2, 4 ),
 ( 0.008988604078116378682, 0.01001254935948934707, 0.01103649464086231546 ),
 .UNSPECIFIED. ) ;
#7480 = CARTESIAN_POINT ( 'NONE',  ( -26.79131905728310059, 51.52708333237728056, -6.403925809002825709 ) ) ;
#7481 = CARTESIAN_POINT ( 'NONE',  ( -25.17020516978313083, 53.80208333237728624, -3.596074190997380349 ) ) ;
#7482 = CARTESIAN_POINT ( 'NONE',  ( 22.11805565807571128, 22.55986279155152374, 12.00579112326941988 ) ) ;
#7483 = CARTESIAN_POINT ( 'NONE',  ( -25.98076211353311393, 52.82499999999986784, -2.690598923241634743 ) ) ;
#7484 = VECTOR ( 'NONE', #3669, 1000.000000000000114 ) ;
#7485 = ORIENTED_EDGE ( 'NONE', *, *, #3909, .T. ) ;
#7486 = EDGE_CURVE ( 'NONE', #6840, #10326, #10097, .T. ) ;
#7487 = ORIENTED_EDGE ( 'NONE', *, *, #457, .F. ) ;
#7488 = VERTEX_POINT ( 'NONE', #3314 ) ;
#7489 = CARTESIAN_POINT ( 'NONE',  ( 4.211140560182196957, -2.431303136016555122, -3.745885042887436622 ) ) ;
#7490 = ORIENTED_EDGE ( 'NONE', *, *, #1729, .T. ) ;
#7491 = EDGE_CURVE ( 'NONE', #4045, #1489, #4802, .T. ) ;
#7492 = CARTESIAN_POINT ( 'NONE',  ( 29.49999999999999645, -3.999999999999983569, 11.65000000000000391 ) ) ;
#7493 = ORIENTED_EDGE ( 'NONE', *, *, #4200, .T. ) ;
#7494 = CARTESIAN_POINT ( 'NONE',  ( 17.45361707773674809, 17.49611573659335662, 12.09524845743996657 ) ) ;
#7495 = CIRCLE ( 'NONE', #9450, 3.299999999999999822 ) ;
#7496 = CARTESIAN_POINT ( 'NONE',  ( -4.000000000000000888, 1.563622288139195238, -0.2253451193528307472 ) ) ;
#7497 = DIRECTION ( 'NONE',  ( 0.000000000000000000, -1.000000000000000000, 1.345283343056720273E-15 ) ) ;
#7498 = CARTESIAN_POINT ( 'NONE',  ( 15.17335179141131185, 18.36218211452176519, 12.24278471274156388 ) ) ;
#7499 = EDGE_CURVE ( 'NONE', #4305, #8252, #4265, .T. ) ;
#7500 =( LENGTH_UNIT ( ) NAMED_UNIT ( * ) SI_UNIT ( .MILLI., .METRE. ) );
#7501 = CARTESIAN_POINT ( 'NONE',  ( -27.98076211353308551, 56.08556146700746581, -4.543501304393035234 ) ) ;
#7502 = DIRECTION ( 'NONE',  ( -1.000000000000000000, 0.000000000000000000, 0.000000000000000000 ) ) ;
#7503 = DIRECTION ( 'NONE',  ( 2.775557561562891351E-17, 1.000000000000000000, -8.326672684688671588E-17 ) ) ;
#7504 = VERTEX_POINT ( 'NONE', #4320 ) ;
#7505 = CARTESIAN_POINT ( 'NONE',  ( 0.06616922564517314920, 33.50000000000000000, 15.90405841526694175 ) ) ;
#7506 = VERTEX_POINT ( 'NONE', #6700 ) ;
#7507 = ADVANCED_FACE ( 'NONE', ( #3430 ), #6454, .F. ) ;
#7508 = ADVANCED_FACE ( 'NONE', ( #10866 ), #4989, .T. ) ;
#7509 = CARTESIAN_POINT ( 'NONE',  ( 20.68923198420054987, 16.84571637733143490, 12.94889058896590583 ) ) ;
#7510 = DIRECTION ( 'NONE',  ( 0.000000000000000000, -9.783878858594328898E-16, -1.000000000000000000 ) ) ;
#7511 = DIRECTION ( 'NONE',  ( 0.000000000000000000, 0.000000000000000000, -1.000000000000000000 ) ) ;
#7512 = CARTESIAN_POINT ( 'NONE',  ( -31.74999999999995737, 3.061616997868384127E-16, -2.500000000000000888 ) ) ;
#7513 = CARTESIAN_POINT ( 'NONE',  ( -1.720978244806803170, 28.18544433887405987, 14.37719158473306713 ) ) ;
#7514 = DIRECTION ( 'NONE',  ( -1.000000000000000000, 0.000000000000000000, 0.000000000000000000 ) ) ;
#7515 = ORIENTED_EDGE ( 'NONE', *, *, #867, .T. ) ;
#7516 = CARTESIAN_POINT ( 'NONE',  ( 25.49999999999999645, -3.999999999999983569, 11.65000000000000746 ) ) ;
#7517 = ORIENTED_EDGE ( 'NONE', *, *, #8232, .T. ) ;
#7518 = EDGE_LOOP ( 'NONE', ( #6784, #3288 ) ) ;
#7519 = VECTOR ( 'NONE', #97, 1000.000000000000000 ) ;
#7520 = CARTESIAN_POINT ( 'NONE',  ( 21.21106610644839208, 53.49999999999983658, 2.500000000000000000 ) ) ;
#7521 = CARTESIAN_POINT ( 'NONE',  ( -27.98076211353308551, 54.72083333142136041, -3.845299461620869330 ) ) ;
#7522 = CARTESIAN_POINT ( 'NONE',  ( 34.86967549602668015, 3.020777328503463366, -3.237032597732066641 ) ) ;
#7523 = DIRECTION ( 'NONE',  ( 6.098637220230963674E-17, -1.000000000000000000, 0.000000000000000000 ) ) ;
#7524 = EDGE_CURVE ( 'NONE', #4598, #8370, #3812, .T. ) ;
#7525 = ADVANCED_FACE ( 'NONE', ( #5003 ), #493, .T. ) ;
#7526 = CARTESIAN_POINT ( 'NONE',  ( 34.89248166448386002, 2.744837293030727210, 3.511881795860531952 ) ) ;
#7527 = CARTESIAN_POINT ( 'NONE',  ( -27.60187600103308370, 50.76874999904395480, -5.000000000000103029 ) ) ;
#7528 = VECTOR ( 'NONE', #1152, 999.9999999999998863 ) ;
#7529 = CARTESIAN_POINT ( 'NONE',  ( 24.49999999999999289, -1.232050807568863426, -4.999999999999992895 ) ) ;
#7530 = CARTESIAN_POINT ( 'NONE',  ( 4.000000000000000000, -1.700175430507292473, -3.320327275037661785 ) ) ;
#7531 = ORIENTED_EDGE ( 'NONE', *, *, #1533, .T. ) ;
#7532 = AXIS2_PLACEMENT_3D ( 'NONE', #8144, #3918, #8193 ) ;
#7533 = CARTESIAN_POINT ( 'NONE',  ( -4.197393957002303999, -7.773935952363655451E-14, -3.503767560748929810 ) ) ;
#7534 = CARTESIAN_POINT ( 'NONE',  ( -27.98076211353308551, 53.99166666666652503, -6.154700538379338504 ) ) ;
#7535 = VECTOR ( 'NONE', #1275, 1000.000000000000000 ) ;
#7536 = DIRECTION ( 'NONE',  ( 2.775557561562891351E-17, 1.000000000000000000, -8.326672684688671588E-17 ) ) ;
#7537 = CARTESIAN_POINT ( 'NONE',  ( -24.35964822603314772, 54.67708333237728624, -5.935950539335252074 ) ) ;
#7538 = CIRCLE ( 'NONE', #3820, 2.767949192431121919 ) ;
#7539 = CARTESIAN_POINT ( 'NONE',  ( 22.82387490247590733, 19.65457484615246386, 12.00579112326941988 ) ) ;
#7540 = SHAPE_REPRESENTATION ( 'BR-590', ( #821, #5102, #298, #4400, #4206, #2620, #4022, #9350, #1542, #8650, #2431, #5457, #5801, #10418 ), #3505 ) ;
#7541 = CARTESIAN_POINT ( 'NONE',  ( -23.98076211353314235, 51.65833333333319644, -6.154700538379337615 ) ) ;
#7542 = AXIS2_PLACEMENT_3D ( 'NONE', #7835, #2784, #5121 ) ;
#7543 = ORIENTED_EDGE ( 'NONE', *, *, #10008, .T. ) ;
#7544 = PRESENTATION_STYLE_ASSIGNMENT (( #7763 ) ) ;
#7545 = VERTEX_POINT ( 'NONE', #10053 ) ;
#7546 = EDGE_LOOP ( 'NONE', ( #1645, #10948, #8710, #8011, #6006, #9941 ) ) ;
#7547 = DIRECTION ( 'NONE',  ( -1.000000000000000000, -0.000000000000000000, -0.000000000000000000 ) ) ;
#7548 = ORIENTED_EDGE ( 'NONE', *, *, #73, .F. ) ;
#7549 = DIRECTION ( 'NONE',  ( -0.000000000000000000, -0.000000000000000000, -1.000000000000000000 ) ) ;
#7550 = CARTESIAN_POINT ( 'NONE',  ( 3.434752482434078047E-15, 1.061650767297805942E-14, 4.999999999999999112 ) ) ;
#7551 = AXIS2_PLACEMENT_3D ( 'NONE', #10474, #5416, #2920 ) ;
#7552 = EDGE_LOOP ( 'NONE', ( #5825, #6589 ) ) ;
#7553 = CARTESIAN_POINT ( 'NONE',  ( 17.86810043078960319, 17.16701444005803268, 12.06109941161078325 ) ) ;
#7554 =( LENGTH_UNIT ( ) NAMED_UNIT ( * ) SI_UNIT ( .MILLI., .METRE. ) );
#7555 = AXIS2_PLACEMENT_3D ( 'NONE', #10313, #5367, #8750 ) ;
#7556 = CARTESIAN_POINT ( 'NONE',  ( 34.99999999999987210, 1.000000000000001332, -11.50000000000000711 ) ) ;
#7557 = DIRECTION ( 'NONE',  ( 0.000000000000000000, 1.000000000000000000, 0.000000000000000000 ) ) ;
#7558 = CARTESIAN_POINT ( 'NONE',  ( 17.39179625728592882, 16.28601130006924791, 12.04260150961189524 ) ) ;
#7559 = DIRECTION ( 'NONE',  ( -0.000000000000000000, -0.000000000000000000, -1.000000000000000000 ) ) ;
#7560 = CARTESIAN_POINT ( 'NONE',  ( -27.98076211353308551, 54.60416666475469327, -6.154700538379338504 ) ) ;
#7561 = CYLINDRICAL_SURFACE ( 'NONE', #4290, 4.999999999999997335 ) ;
#7562 = EDGE_LOOP ( 'NONE', ( #6648, #809, #3388, #3207, #2942, #8280, #768, #2123 ) ) ;
#7563 = ORIENTED_EDGE ( 'NONE', *, *, #3035, .T. ) ;
#7564 = CARTESIAN_POINT ( 'NONE',  ( 3.500000000000005773, 31.44974746830583356, 14.67187500000000178 ) ) ;
#7565 = ORIENTED_EDGE ( 'NONE', *, *, #9663, .F. ) ;
#7566 =( REPRESENTATION_RELATIONSHIP ('NONE','NONE', #7540, #75 ) REPRESENTATION_RELATIONSHIP_WITH_TRANSFORMATION ( #1322 )SHAPE_REPRESENTATION_RELATIONSHIP( ) );
#7567 = CARTESIAN_POINT ( 'NONE',  ( 22.13583660366028738, 22.61346442202890472, 13.00425721518307753 ) ) ;
#7568 = ADVANCED_FACE ( 'NONE', ( #5618 ), #252, .T. ) ;
#7569 = EDGE_CURVE ( 'NONE', #1334, #7218, #774, .T. ) ;
#7570 = CARTESIAN_POINT ( 'NONE',  ( 16.50280774463635680, 17.03272616129868666, 12.11810441208646338 ) ) ;
#7571 = PLANE ( 'NONE',  #1267 ) ;
#7572 = CARTESIAN_POINT ( 'NONE',  ( -26.77929575296436582, 57.38439079953180766, -3.163742677926416835 ) ) ;
#7573 = CARTESIAN_POINT ( 'NONE',  ( 2.527408190673965382, 29.03063531971243449, 14.76781658473306535 ) ) ;
#7574 = PRODUCT_DEFINITION_FORMATION_WITH_SPECIFIED_SOURCE ( 'ANY', '', #5016, .NOT_KNOWN. ) ;
#7575 = CARTESIAN_POINT ( 'NONE',  ( 34.99999999999999289, -3.999999999999993339, 12.14999999999999680 ) ) ;
#7576 = CARTESIAN_POINT ( 'NONE',  ( 2.000000000000000000, 1.773042676681340524, -2.059984127722458425E-15 ) ) ;
#7577 = CYLINDRICAL_SURFACE ( 'NONE', #10251, 20.00000000000000355 ) ;
#7578 = VERTEX_POINT ( 'NONE', #7273 ) ;
#7579 = EDGE_LOOP ( 'NONE', ( #4998, #6319, #5157, #3299, #7025, #5795, #3055 ) ) ;
#7580 = CARTESIAN_POINT ( 'NONE',  ( 21.21106610644839208, 56.49999999999984368, 2.500000000000000000 ) ) ;
#7581 = CARTESIAN_POINT ( 'NONE',  ( -26.98076211353309972, 54.54583333142136325, -6.732050807568954909 ) ) ;
#7582 = PRODUCT_DEFINITION_SHAPE ( 'NONE', 'NONE',  #3420 ) ;
#7583 = AXIS2_PLACEMENT_3D ( 'NONE', #4647, #8032, #7247 ) ;
#7584 = AXIS2_PLACEMENT_3D ( 'NONE', #386, #2742, #10346 ) ;
#7585 = CARTESIAN_POINT ( 'NONE',  ( 18.79784185921769790, 16.99560944861731215, 12.01584860934582366 ) ) ;
#7586 = UNCERTAINTY_MEASURE_WITH_UNIT (LENGTH_MEASURE( 1.000000000000000082E-05 ), #8442, 'distance_accuracy_value', 'NONE');
#7587 = DIRECTION ( 'NONE',  ( -0.000000000000000000, -0.000000000000000000, 1.000000000000000000 ) ) ;
#7588 = DIRECTION ( 'NONE',  ( 0.000000000000000000, 0.000000000000000000, 1.000000000000000000 ) ) ;
#7589 = CARTESIAN_POINT ( 'NONE',  ( -24.35964822603314772, 53.16041666571062763, -4.064049460664953983 ) ) ;
#7590 = DIRECTION ( 'NONE',  ( 0.000000000000000000, 0.000000000000000000, 1.000000000000000000 ) ) ;
#7591 = DIRECTION ( 'NONE',  ( 0.000000000000000000, 0.000000000000000000, -1.000000000000000000 ) ) ;
#7592 = CYLINDRICAL_SURFACE ( 'NONE', #9140, 4.250000000000000000 ) ;
#7593 = VERTEX_POINT ( 'NONE', #6546 ) ;
#7594 = CONICAL_SURFACE ( 'NONE', #791, 1.615000000000000213, 0.9599310885968811435 ) ;
#7595 = DIRECTION ( 'NONE',  ( 1.000000000000000000, 0.000000000000000000, 0.000000000000000000 ) ) ;
#7596 = PLANE ( 'NONE',  #9907 ) ;
#7597 = CARTESIAN_POINT ( 'NONE',  ( -26.79131905728310059, 54.32708333237727771, -6.403925809002825709 ) ) ;
#7598 = ADVANCED_FACE ( 'NONE', ( #9943 ), #5719, .T. ) ;
#7599 = CYLINDRICAL_SURFACE ( 'NONE', #3468, 1.650000000000000355 ) ;
#7600 =( GEOMETRIC_REPRESENTATION_CONTEXT ( 3 ) GLOBAL_UNCERTAINTY_ASSIGNED_CONTEXT ( ( #8970 ) ) GLOBAL_UNIT_ASSIGNED_CONTEXT ( ( #9737, #6121, #9570 ) ) REPRESENTATION_CONTEXT ( 'NONE', 'WORKASPACE' ) );
#7601 =( GEOMETRIC_REPRESENTATION_CONTEXT ( 3 ) GLOBAL_UNCERTAINTY_ASSIGNED_CONTEXT ( ( #1084 ) ) GLOBAL_UNIT_ASSIGNED_CONTEXT ( ( #3943, #6493, #1609 ) ) REPRESENTATION_CONTEXT ( 'NONE', 'WORKASPACE' ) );
#7602 = VECTOR ( 'NONE', #10198, 1000.000000000000000 ) ;
#7603 = CARTESIAN_POINT ( 'NONE',  ( -4.000000000000000000, 2.309401076758498483, -5.000000000000000000 ) ) ;
#7604 = CARTESIAN_POINT ( 'NONE',  ( -25.98076211353311393, 53.52499999999986358, -2.690598923241634743 ) ) ;
#7605 = EDGE_LOOP ( 'NONE', ( #4702, #8839, #5506, #9724, #7969, #7515 ) ) ;
#7606 = CARTESIAN_POINT ( 'NONE',  ( 29.50000000000000711, -3.999999999999989786, -4.999999999999999112 ) ) ;
#7607 = ORIENTED_EDGE ( 'NONE', *, *, #4082, .F. ) ;
#7608 = ORIENTED_EDGE ( 'NONE', *, *, #6200, .T. ) ;
#7609 = DIRECTION ( 'NONE',  ( -0.000000000000000000, -1.000000000000000000, -0.000000000000000000 ) ) ;
#7610 = VERTEX_POINT ( 'NONE', #10668 ) ;
#7611 = CARTESIAN_POINT ( 'NONE',  ( 0.000000000000000000, 0.000000000000000000, -0.3080913168122742518 ) ) ;
#7612 = ORIENTED_EDGE ( 'NONE', *, *, #6147, .F. ) ;
#7613 = CARTESIAN_POINT ( 'NONE',  ( 22.66010611969070965, 19.57566612754892432, 11.00732503135576401 ) ) ;
#7614 = CARTESIAN_POINT ( 'NONE',  ( 2.982579934988239145, 3.876582599186223277, -0.2855619784720935250 ) ) ;
#7615 = CARTESIAN_POINT ( 'NONE',  ( -4.000000000000000000, 0.9868501483902560878, -0.09357334158579519445 ) ) ;
#7616 =( BOUNDED_CURVE ( )  B_SPLINE_CURVE ( 2, ( #8801, #8863, #1184, #4587, #9689, #2082, #6131, #9522, #4639 ),
 .UNSPECIFIED., .F., .F. ) 
 B_SPLINE_CURVE_WITH_KNOTS ( ( 3, 2, 2, 2, 3 ),
 ( 0.08333333333333331483, 0.09259259259259258745, 0.1111111111111111049, 0.1296296296296296224, 0.1388888888888888951 ),
 .UNSPECIFIED. ) 
 CURVE ( )  GEOMETRIC_REPRESENTATION_ITEM ( )  RATIONAL_B_SPLINE_CURVE ( ( 0.9330127018922192983, 0.9330127018922191873, 1.000000000000000000, 0.8660254037844387076, 1.000000000000000000, 0.8660254037844387076, 1.000000000000000000, 0.9330127018922191873, 0.9330127018922192983 ) ) 
 REPRESENTATION_ITEM ( '' )  );
#7617 = DIRECTION ( 'NONE',  ( 0.000000000000000000, 0.000000000000000000, -1.000000000000000000 ) ) ;
#7618 = CARTESIAN_POINT ( 'NONE',  ( 23.64018263364375017, 19.06693133664117212, 11.95042449705224819 ) ) ;
#7619 = CARTESIAN_POINT ( 'NONE',  ( 25.49999999999999645, -3.999999999999986233, -4.999999999999992006 ) ) ;
#7620 = CARTESIAN_POINT ( 'NONE',  ( -27.60187600103308014, 50.30208333237727913, -4.064049460664955760 ) ) ;
#7621 = CARTESIAN_POINT ( 'NONE',  ( -4.197393957002303999, -7.773935952363655451E-14, -3.503767560748929810 ) ) ;
#7622 = ORIENTED_EDGE ( 'NONE', *, *, #1271, .T. ) ;
#7623 = DIRECTION ( 'NONE',  ( 0.000000000000000000, 0.000000000000000000, -1.000000000000000000 ) ) ;
#7624 = ORIENTED_EDGE ( 'NONE', *, *, #9983, .F. ) ;
#7625 = CARTESIAN_POINT ( 'NONE',  ( 3.472591809326047052, 31.51591669395100936, 14.92406658473306713 ) ) ;
#7626 = ORIENTED_EDGE ( 'NONE', *, *, #5148, .F. ) ;
#7627 = EDGE_CURVE ( 'NONE', #10425, #4665, #6286, .T. ) ;
#7628 = CARTESIAN_POINT ( 'NONE',  ( 22.89753608554585540, 18.38182967998604056, 12.94889058896590583 ) ) ;
#7629 = CARTESIAN_POINT ( 'NONE',  ( 17.02848097699435215, 16.52496068989110967, 12.06979569234921890 ) ) ;
#7630 = CARTESIAN_POINT ( 'NONE',  ( -21.21106610644865498, 16.50000000000026290, -2.500000000000000000 ) ) ;
#7631 = CARTESIAN_POINT ( 'NONE',  ( -24.35964822603314417, 49.71874999904395054, -5.000000000000103029 ) ) ;
#7632 = CARTESIAN_POINT ( 'NONE',  ( -1.767766952966370209, 28.23223304703362402, 14.12500000000000355 ) ) ;
#7633 = CARTESIAN_POINT ( 'NONE',  ( 0.000000000000000000, 0.000000000000000000, 0.000000000000000000 ) ) ;
#7634 = CARTESIAN_POINT ( 'NONE',  ( -25.98076211353310683, 55.53749999808803040, -3.000000000000132339 ) ) ;
#7635 = DIRECTION ( 'NONE',  ( 0.000000000000000000, 0.000000000000000000, 1.000000000000000000 ) ) ;
#7636 = EDGE_CURVE ( 'NONE', #647, #1508, #9833, .T. ) ;
#7637 = ORIENTED_EDGE ( 'NONE', *, *, #1388, .T. ) ;
#7638 = EDGE_LOOP ( 'NONE', ( #3110, #3941, #2886 ) ) ;
#7639 = EDGE_CURVE ( 'NONE', #1168, #5275, #7179, .T. ) ;
#7640 = CARTESIAN_POINT ( 'NONE',  ( 1.655952806101427033, -3.662737355149048302, -1.182683869819604841E-14 ) ) ;
#7641 = CARTESIAN_POINT ( 'NONE',  ( 25.49999999999999645, -3.999999999999986233, -4.999999999999992006 ) ) ;
#7642 = CARTESIAN_POINT ( 'NONE',  ( 19.13264607096459002, 17.09257730534942965, 12.00833071292064425 ) ) ;
#7643 = CARTESIAN_POINT ( 'NONE',  ( -2.500000000000005773, 29.99999999999999645, 16.46875000000000355 ) ) ;
#7644 = CARTESIAN_POINT ( 'NONE',  ( 0.5636800770130377947, 4.293361309317166530, -3.531542292954102713 ) ) ;
#7645 = CARTESIAN_POINT ( 'NONE',  ( -26.79131905728310059, 53.45208333237728482, -6.403925809002825709 ) ) ;
#7646 = DIRECTION ( 'NONE',  ( 0.000000000000000000, 0.000000000000000000, 1.000000000000000000 ) ) ;
#7647 = DIRECTION ( 'NONE',  ( 0.000000000000000000, 1.000000000000000000, 0.000000000000000000 ) ) ;
#7648 = CARTESIAN_POINT ( 'NONE',  ( 3.679171394226031122, 2.494631558665830973, -0.3503314178412474389 ) ) ;
#7649 = EDGE_CURVE ( 'NONE', #5796, #9475, #2377, .T. ) ;
#7650 = ORIENTED_EDGE ( 'NONE', *, *, #1449, .T. ) ;
#7651 = CARTESIAN_POINT ( 'NONE',  ( 29.49999999999999645, 2.000000000000001776, -12.49999999999999822 ) ) ;
#7652 = LINE ( 'NONE', #5044, #4428 ) ;
#7653 = EDGE_CURVE ( 'NONE', #1662, #1634, #2283, .T. ) ;
#7654 = EDGE_CURVE ( 'NONE', #9249, #4777, #9049, .T. ) ;
#7655 = CARTESIAN_POINT ( 'NONE',  ( -24.35964822603314417, 54.79374999904394627, -5.000000000000103029 ) ) ;
#7656 = CARTESIAN_POINT ( 'NONE',  ( -25.98076211353310683, 55.49374999904395622, -6.871901078670399343 ) ) ;
#7657 = AXIS2_PLACEMENT_3D ( 'NONE', #5582, #3857, #2140 ) ;
#7658 = CIRCLE ( 'NONE', #9250, 24.99999999999999645 ) ;
#7659 = CARTESIAN_POINT ( 'NONE',  ( 34.99999999999987210, 16.00000000000000355, 1.499999999999902522 ) ) ;
#7660 = CARTESIAN_POINT ( 'NONE',  ( -23.98076211353314235, 50.89999999999986358, -5.000000000000103029 ) ) ;
#7661 = EDGE_LOOP ( 'NONE', ( #4329, #10827, #9448, #9282, #6664 ) ) ;
#7662 = VERTEX_POINT ( 'NONE', #1549 ) ;
#7663 = DIRECTION ( 'NONE',  ( 0.000000000000000000, -0.000000000000000000, 1.000000000000000000 ) ) ;
#7664 = ORIENTED_EDGE ( 'NONE', *, *, #4025, .T. ) ;
#7665 = CARTESIAN_POINT ( 'NONE',  ( 23.05579831881754416, 20.86490736922957367, 14.50000000000000000 ) ) ;
#7666 = DIRECTION ( 'NONE',  ( 0.000000000000000000, 0.000000000000000000, 1.000000000000000000 ) ) ;
#7667 = ORIENTED_EDGE ( 'NONE', *, *, #1546, .F. ) ;
#7668 =( BOUNDED_CURVE ( )  B_SPLINE_CURVE ( 2, ( #3749, #5315, #1251, #2924, #4643 ),
 .UNSPECIFIED., .F., .F. ) 
 B_SPLINE_CURVE_WITH_KNOTS ( ( 3, 2, 3 ),
 ( 0.000000000000000000, 0.01851851851851852096, 0.02777777777777775542 ),
 .UNSPECIFIED. ) 
 CURVE ( )  GEOMETRIC_REPRESENTATION_ITEM ( )  RATIONAL_B_SPLINE_CURVE ( ( 1.000000000000000000, 0.8660254037844387076, 1.000000000000000000, 0.9330127018922195203, 0.9330127018922194093 ) ) 
 REPRESENTATION_ITEM ( '' )  );
#7669 = CARTESIAN_POINT ( 'NONE',  ( 20.17304365239387565, 21.99495017005343200, 12.00579112326981068 ) ) ;
#7670 = DIRECTION ( 'NONE',  ( -1.000000000000000000, 0.000000000000000000, 0.000000000000000000 ) ) ;
#7671 = CARTESIAN_POINT ( 'NONE',  ( 0.000000000000000000, -3.031088913245550298, -1.749999999999972911 ) ) ;
#7672 = EDGE_CURVE ( 'NONE', #9151, #3442, #5053, .T. ) ;
#7673 = CARTESIAN_POINT ( 'NONE',  ( 22.44460225903107187, 18.20165426066020942, 10.95195840513859231 ) ) ;
#7674 = CARTESIAN_POINT ( 'NONE',  ( -4.000000000000000000, -2.309401076758515803, -0.4999999999999995559 ) ) ;
#7675 = CARTESIAN_POINT ( 'NONE',  ( 8.673617379884035472E-16, 4.618802153517012954, 0.000000000000000000 ) ) ;
#7676 = CARTESIAN_POINT ( 'NONE',  ( -25.98076211353311393, 55.88749999808803182, -7.309401076758571314 ) ) ;
#7677 = CYLINDRICAL_SURFACE ( 'NONE', #6950, 30.00000000000000000 ) ;
#7678 = ORIENTED_EDGE ( 'NONE', *, *, #5726, .F. ) ;
#7679 = CARTESIAN_POINT ( 'NONE',  ( 34.99999999999987210, -3.999999999999989786, -2.850000000000007194 ) ) ;
#7680 = PRODUCT ( 'socket head cap screw_iso_ISO 4762 M4 x 8 - 8N', 'socket head cap screw_iso_ISO 4762 M4 x 8 - 8N', '', ( #5992 ) ) ;
#7681 = ORIENTED_EDGE ( 'NONE', *, *, #6099, .T. ) ;
#7682 = CARTESIAN_POINT ( 'NONE',  ( -3.456897879362375470, 29.45240795142740353, 16.49922112211940117 ) ) ;
#7683 = VERTEX_POINT ( 'NONE', #814 ) ;
#7684 = CARTESIAN_POINT ( 'NONE',  ( 21.30711663910541276, 17.34296610691914253, 11.95042449705224819 ) ) ;
#7685 =( BOUNDED_CURVE ( )  B_SPLINE_CURVE ( 2, ( #4135, #3307, #7303, #1369, #8146, #10696, #3088, #2256, #8194, #571, #5860, #9297, #10308, #10088, #1760, #2476, #5093, #8640, #2703, #8473, #5914, #9412, #5972, #8410, #9243, #857, #8532, #10254, #10194, #9362, #1696, #2593, #4258, #5151, #909, #6028, #3365, #1021, #7643, #19, #1860 ),
 .UNSPECIFIED., .F., .T. ) 
 B_SPLINE_CURVE_WITH_KNOTS ( ( 3, 2, 2, 2, 2, 2, 2, 2, 2, 2, 2, 2, 2, 2, 2, 2, 2, 2, 2, 2, 3 ),
 ( 0.000000000000000000, 0.04166666666666666435, 0.08333333333333332871, 0.1250000000000000000, 0.1666666666666666574, 0.2083333333333333148, 0.2500000000000000000, 0.2916666666666666852, 0.3333333333333333148, 0.3750000000000000000, 0.4166666666666666297, 0.4583333333333333148, 0.5000000000000000000, 0.5416666666666666297, 0.5833333333333333703, 0.6250000000000000000, 0.6666666666666666297, 0.7083333333333334814, 0.7500000000000000000, 0.7916666666666666297, 0.8001047462599640836 ),
 .UNSPECIFIED. ) 
 CURVE ( )  GEOMETRIC_REPRESENTATION_ITEM ( )  RATIONAL_B_SPLINE_CURVE ( ( 1.000000000000000000, 0.9238795325112867385, 1.000000000000000000, 0.9238795325112867385, 1.000000000000000000, 0.9238795325112867385, 1.000000000000000000, 0.9238795325112867385, 1.000000000000000000, 0.9238795325112867385, 1.000000000000000000, 0.9238795325112867385, 1.000000000000000000, 0.9238795325112867385, 1.000000000000000000, 0.9238795325112867385, 1.000000000000000000, 0.9238795325112867385, 1.000000000000000000, 0.9238795325112867385, 1.000000000000000000, 0.9238795325112867385, 1.000000000000000000, 0.9238795325112867385, 1.000000000000000000, 0.9238795325112867385, 1.000000000000000000, 0.9238795325112867385, 1.000000000000000000, 0.9238795325112867385, 1.000000000000000000, 0.9238795325112867385, 1.000000000000000000, 0.9238795325112867385, 1.000000000000000000, 0.9238795325112867385, 1.000000000000000000, 0.9238795325112867385, 1.000000000000000000, 0.9845845464796294522, 0.9754127805002987817 ) ) 
 REPRESENTATION_ITEM ( '' )  );
#7686 =( NAMED_UNIT ( * ) PLANE_ANGLE_UNIT ( ) SI_UNIT ( $, .RADIAN. ) );
#7687 = CARTESIAN_POINT ( 'NONE',  ( 15.87890888817147150, 17.65662501776163040, 12.17661548709639341 ) ) ;
#7688 = CARTESIAN_POINT ( 'NONE',  ( 17.13192716875488131, 17.81782029955189728, 12.12541829646253078 ) ) ;
#7689 = CARTESIAN_POINT ( 'NONE',  ( -27.60187600103308370, 52.86874999904394912, -5.000000000000103029 ) ) ;
#7690 = ADVANCED_FACE ( 'NONE', ( #1889 ), #1140, .F. ) ;
#7691 = CARTESIAN_POINT ( 'NONE',  ( 1.035533905932737975, 32.50000000000000711, 14.82812500000000178 ) ) ;
#7692 = CARTESIAN_POINT ( 'NONE',  ( -9.167668597118891028E-15, -10.00000000000000000, 15.49999999999998757 ) ) ;
#7693 = CARTESIAN_POINT ( 'NONE',  ( 25.98076211353311749, 56.49999999999984368, 10.00000000000000178 ) ) ;
#7694 = ORIENTED_EDGE ( 'NONE', *, *, #8466, .F. ) ;
#7695 = VERTEX_POINT ( 'NONE', #989 ) ;
#7696 = B_SPLINE_CURVE_WITH_KNOTS ( 'NONE', 3,
 ( #1462, #4012, #3180, #2344, #9116, #8474, #4982, #8411, #10978, #7526, #858, #4868, #1584, #7359, #4085, #2419 ),
 .UNSPECIFIED., .F., .F.,
 ( 4, 2, 2, 2, 2, 2, 2, 4 ),
 ( 0.000000000000000000, 0.0005875779155018995932, 0.001175155831003799186, 0.001762733746505698454, 0.002350311662007598373, 0.002937889577509498074, 0.003525467493011396041, 0.004700623324015193276 ),
 .UNSPECIFIED. ) ;
#7697 = CARTESIAN_POINT ( 'NONE',  ( -26.98076211353309972, 51.83333333333319359, -6.732050807568954909 ) ) ;
#7698 = CARTESIAN_POINT ( 'NONE',  ( 34.90224802882303834, 2.616310811731262120, -3.667896704194530511 ) ) ;
#7699 = CARTESIAN_POINT ( 'NONE',  ( -25.98076211353311393, 55.88749999808803182, -7.000000000000072831 ) ) ;
#7700 = CARTESIAN_POINT ( 'NONE',  ( -25.98076211353324894, 4.999999999999997335, 2.500000000000000000 ) ) ;
#7701 = CARTESIAN_POINT ( 'NONE',  ( -24.35964822603314417, 55.31874999904395196, -5.000000000000103029 ) ) ;
#7702 = EDGE_CURVE ( 'NONE', #3831, #1419, #2209, .T. ) ;
#7703 = EDGE_CURVE ( 'NONE', #10716, #1715, #10273, .T. ) ;
#7704 = DIRECTION ( 'NONE',  ( 0.000000000000000000, 0.000000000000000000, 1.000000000000000000 ) ) ;
#7705 = LINE ( 'NONE', #6803, #10376 ) ;
#7706 = CARTESIAN_POINT ( 'NONE',  ( 2.171643655288379993, -3.365003104552334978, -1.195831703456429434E-14 ) ) ;
#7707 = ORIENTED_EDGE ( 'NONE', *, *, #6268, .T. ) ;
#7708 = DIRECTION ( 'NONE',  ( 1.000000000000000000, -0.000000000000000000, 1.156482317317871478E-16 ) ) ;
#7709 = CARTESIAN_POINT ( 'NONE',  ( -25.98076211353311393, 53.87499999999986500, -7.000000000000072831 ) ) ;
#7710 = CARTESIAN_POINT ( 'NONE',  ( -25.98076211353310683, 52.86874999904393491, -6.871901078670399343 ) ) ;
#7711 = ADVANCED_FACE ( 'NONE', ( #4220 ), #5115, .F. ) ;
#7712 = CARTESIAN_POINT ( 'NONE',  ( -25.98076211353311393, 50.72499999999985931, -3.000000000000132783 ) ) ;
#7713 = EDGE_CURVE ( 'NONE', #1015, #1493, #9323, .T. ) ;
#7714 = PLANE ( 'NONE',  #5548 ) ;
#7715 = DIRECTION ( 'NONE',  ( -0.000000000000000000, -0.000000000000000000, -1.000000000000000000 ) ) ;
#7716 = CONICAL_SURFACE ( 'NONE', #8229, 1.649999999999998579, 1.029744258676653423 ) ;
#7717 = EDGE_LOOP ( 'NONE', ( #2545, #4723, #9545 ) ) ;
#7718 = AXIS2_PLACEMENT_3D ( 'NONE', #2551, #7549, #8435 ) ;
#7719 = VERTEX_POINT ( 'NONE', #7665 ) ;
#7720 = DIRECTION ( 'NONE',  ( -0.000000000000000000, -0.000000000000000000, -1.000000000000000000 ) ) ;
#7721 = CARTESIAN_POINT ( 'NONE',  ( 0.000000000000000000, 0.000000000000000000, 0.000000000000000000 ) ) ;
#7722 = DIRECTION ( 'NONE',  ( 1.000000000000000000, 0.000000000000000000, 0.000000000000000000 ) ) ;
#7723 = ORIENTED_EDGE ( 'NONE', *, *, #6596, .T. ) ;
#7724 = CARTESIAN_POINT ( 'NONE',  ( 23.31827848602400621, 20.57738196266585362, 12.00579112326941988 ) ) ;
#7725 = DIRECTION ( 'NONE',  ( 0.000000000000000000, 0.000000000000000000, 1.000000000000000000 ) ) ;
#7726 = AXIS2_PLACEMENT_3D ( 'NONE', #8820, #2993, #10540 ) ;
#7727 = DIRECTION ( 'NONE',  ( -0.000000000000000000, 0.8660254037844390407, 0.4999999999999993339 ) ) ;
#7728 = CARTESIAN_POINT ( 'NONE',  ( -24.35964822603314417, 50.59374999904394343, -5.000000000000103029 ) ) ;
#7729 = CARTESIAN_POINT ( 'NONE',  ( 16.37803167940877458, 17.15750222652490820, 11.12760988119559258 ) ) ;
#7730 = CARTESIAN_POINT ( 'NONE',  ( 1.449747468305832898, 33.50000000000000000, 16.07812500000000355 ) ) ;
#7731 = CARTESIAN_POINT ( 'NONE',  ( -26.79131905728310059, 50.82708333237727771, -6.403925809002825709 ) ) ;
#7732 = AXIS2_PLACEMENT_3D ( 'NONE', #2343, #8285, #673 ) ;
#7733 = FACE_OUTER_BOUND ( 'NONE', #9435, .T. ) ;
#7734 = ORIENTED_EDGE ( 'NONE', *, *, #5530, .T. ) ;
#7735 = CARTESIAN_POINT ( 'NONE',  ( -25.71445732839318765, 58.97263009590939475, -3.014038965319806973 ) ) ;
#7736 = ORIENTED_EDGE ( 'NONE', *, *, #10223, .T. ) ;
#7737 = CARTESIAN_POINT ( 'NONE',  ( -3.527408190673960053, 31.38357824266065066, 14.14281658473306713 ) ) ;
#7738 = CIRCLE ( 'NONE', #5954, 2.700000000000001066 ) ;
#7739 = VERTEX_POINT ( 'NONE', #10164 ) ;
#7740 = B_SPLINE_CURVE_WITH_KNOTS ( 'NONE', 3,
 ( #2978, #3692, #5361, #7972 ),
 .UNSPECIFIED., .F., .F.,
 ( 4, 4 ),
 ( 2.380739286522876005E-07, 0.002044882221487540584 ),
 .UNSPECIFIED. ) ;
#7741 = CARTESIAN_POINT ( 'NONE',  ( 20.65761543282678758, 16.89116807672653664, 11.95042449705224819 ) ) ;
#7742 = SURFACE_STYLE_FILL_AREA ( #10238 ) ;
#7743 = VECTOR ( 'NONE', #10125, 1000.000000000000000 ) ;
#7744 = CARTESIAN_POINT ( 'NONE',  ( 19.76265562249496099, 16.28401831655332543, 11.95127577209155234 ) ) ;
#7745 = CARTESIAN_POINT ( 'NONE',  ( -25.98076211353311038, 61.49999999999985789, -0.9999999999995021760 ) ) ;
#7747 = CARTESIAN_POINT ( 'NONE',  ( -26.79131905728310059, 50.88541666571061484, -3.596074190997381237 ) ) ;
#7746 = AXIS2_PLACEMENT_3D ( 'NONE', #5691, #4187, #2348 ) ;
#7748 = DIRECTION ( 'NONE',  ( 0.000000000000000000, -0.4999999999999993894, 0.8660254037844389297 ) ) ;
#7749 = DIRECTION ( 'NONE',  ( 0.000000000000000000, 0.000000000000000000, -1.000000000000000000 ) ) ;
#7750 = DIRECTION ( 'NONE',  ( -1.000000000000000000, 0.000000000000000000, -0.000000000000000000 ) ) ;
#7751 = ORIENTED_EDGE ( 'NONE', *, *, #9114, .F. ) ;
#7752 = EDGE_LOOP ( 'NONE', ( #5898, #8495, #7762, #3344 ) ) ;
#7753 = CARTESIAN_POINT ( 'NONE',  ( 29.17190429162963738, 6.999999999999999112, 2.500000000000000000 ) ) ;
#7754 = CARTESIAN_POINT ( 'NONE',  ( 24.30992024302469900, 5.833333333333334814, 2.500000000000000000 ) ) ;
#7755 = CARTESIAN_POINT ( 'NONE',  ( 34.91794119163850496, 2.397787035234374198, -3.994322637888107597 ) ) ;
#7756 = CARTESIAN_POINT ( 'NONE',  ( -27.98076211353308551, 52.70833333333320780, -3.845299461620869330 ) ) ;
#7757 = CARTESIAN_POINT ( 'NONE',  ( -6.259644161404860030E-16, -4.618802153517027165, -5.000000000000000000 ) ) ;
#7758 = CARTESIAN_POINT ( 'NONE',  ( -24.35964822603314772, 53.86041666571062336, -4.064049460664953983 ) ) ;
#7759 = CARTESIAN_POINT ( 'NONE',  ( 2.500000000000000000, 2.357898499370433054, -1.951563910473907981E-15 ) ) ;
#7760 = PLANE ( 'NONE',  #8245 ) ;
#7761 = DIRECTION ( 'NONE',  ( 4.312387734421975126E-17, -0.7071067811865451302, -0.7071067811865500152 ) ) ;
#7762 = ORIENTED_EDGE ( 'NONE', *, *, #4046, .F. ) ;
#7763 = SURFACE_STYLE_USAGE ( .BOTH. , #1932 ) ;
#7764 = CARTESIAN_POINT ( 'NONE',  ( 0.06616922564517249694, 32.50000000000000711, 14.65405841526694353 ) ) ;
#7765 = PRODUCT_DEFINITION ( 'UNKNOWN', '', #8117, #10003 ) ;
#7766 = AXIS2_PLACEMENT_3D ( 'NONE', #1013, #6792, #2519 ) ;
#7767 = MECHANICAL_DESIGN_GEOMETRIC_PRESENTATION_REPRESENTATION (  '', ( #2799 ), #8281 ) ;
#7768 = CARTESIAN_POINT ( 'NONE',  ( 1.035533905932737975, 32.50000000000000711, 16.07812500000000355 ) ) ;
#7769 = EDGE_CURVE ( 'NONE', #6424, #1907, #5058, .T. ) ;
#7770 = CARTESIAN_POINT ( 'NONE',  ( -25.17020516978313083, 54.21041666571061057, -6.403925809002825709 ) ) ;
#7771 = CARTESIAN_POINT ( 'NONE',  ( 2.500000000000000000, -2.357898499370432610, 3.252606517456513302E-15 ) ) ;
#7772 = PRODUCT_DEFINITION_SHAPE ( 'NONE', 'NONE',  #11002 ) ;
#7773 = DIRECTION ( 'NONE',  ( 0.000000000000000000, 0.000000000000000000, -1.000000000000000000 ) ) ;
#7774 = AXIS2_PLACEMENT_3D ( 'NONE', #8621, #1377, #4409 ) ;
#7775 = VECTOR ( 'NONE', #3695, 1000.000000000000000 ) ;
#7776 = CARTESIAN_POINT ( 'NONE',  ( -24.98076211353313170, 54.98333333333319928, -3.267949192431250705 ) ) ;
#7777 = ORIENTED_EDGE ( 'NONE', *, *, #743, .T. ) ;
#7778 = ORIENTED_EDGE ( 'NONE', *, *, #1460, .T. ) ;
#7779 = CARTESIAN_POINT ( 'NONE',  ( 0.000000000000000000, 0.000000000000000000, -2.000000000000000000 ) ) ;
#7780 = ADVANCED_FACE ( 'NONE', ( #6045 ), #5882, .F. ) ;
#7781 = DIRECTION ( 'NONE',  ( -1.000000000000000000, 0.000000000000000000, 0.000000000000000000 ) ) ;
#7782 = APPLICATION_PROTOCOL_DEFINITION ( 'draft international standard', 'automotive_design', 1998, #1750 ) ;
#7783 = ORIENTED_EDGE ( 'NONE', *, *, #9838, .F. ) ;
#7784 = AXIS2_PLACEMENT_3D ( 'NONE', #4623, #8008, #380 ) ;
#7785 = PRESENTATION_LAYER_ASSIGNMENT (  '', '', ( #6889 ) ) ;
#7786 = CARTESIAN_POINT ( 'NONE',  ( 4.211140560182196957, 2.431303136016536470, -3.745885042887433514 ) ) ;
#7787 = CARTESIAN_POINT ( 'NONE',  ( -25.98076211353311393, 54.22499999999985931, -3.000000000000132339 ) ) ;
#7788 = VECTOR ( 'NONE', #1359, 1000.000000000000000 ) ;
#7789 = APPLICATION_CONTEXT ( 'automotive_design' ) ;
#7790 = CARTESIAN_POINT ( 'NONE',  ( 17.74381166370891449, 16.14600641939347980, 11.01911823137775492 ) ) ;
#7791 = FACE_OUTER_BOUND ( 'NONE', #8336, .T. ) ;
#7792 = CARTESIAN_POINT ( 'NONE',  ( -25.98076211353311393, 53.56874999904394485, -6.871901078670400231 ) ) ;
#7793 = EDGE_CURVE ( 'NONE', #1093, #2280, #5240, .T. ) ;
#7794 = CARTESIAN_POINT ( 'NONE',  ( 29.49999999999999645, -3.999999999999993339, -2.850000000000008082 ) ) ;
#7795 = ORIENTED_EDGE ( 'NONE', *, *, #10155, .F. ) ;
#7796 = FACE_OUTER_BOUND ( 'NONE', #6472, .T. ) ;
#7797 = ORIENTED_EDGE ( 'NONE', *, *, #555, .T. ) ;
#7798 = CIRCLE ( 'NONE', #1221, 4.000000000000000000 ) ;
#7799 = CARTESIAN_POINT ( 'NONE',  ( -2.428085025993349078, 27.47833755768751374, 13.12719158473306535 ) ) ;
#7800 = VERTEX_POINT ( 'NONE', #3386 ) ;
#7801 = CARTESIAN_POINT ( 'NONE',  ( 17.26579466391090634, 16.35877559204224951, 12.05147379044805866 ) ) ;
#7802 = ADVANCED_FACE ( 'NONE', ( #10936 ), #8948, .T. ) ;
#7803 = CARTESIAN_POINT ( 'NONE',  ( 23.54706165660595829, 18.96431965174070555, 11.95042449705224819 ) ) ;
#7804 = CARTESIAN_POINT ( 'NONE',  ( 22.44007493706583745, 19.34731747087121434, 12.00579112326928133 ) ) ;
#7805 = CARTESIAN_POINT ( 'NONE',  ( -24.35964822603314417, 52.51874999904394770, -5.000000000000103029 ) ) ;
#7806 = CARTESIAN_POINT ( 'NONE',  ( 2.500000000000010214, 28.96446609406726225, 14.51562500000000355 ) ) ;
#7807 = CARTESIAN_POINT ( 'NONE',  ( 5.791420021395468964, 3.879972077055416885E-33, -3.168237633705329831E-17 ) ) ;
#7808 = PLANE ( 'NONE',  #9359 ) ;
#7809 = VERTEX_POINT ( 'NONE', #10216 ) ;
#7810 = ORIENTED_EDGE ( 'NONE', *, *, #4190, .F. ) ;
#7811 = EDGE_CURVE ( 'NONE', #1566, #1959, #7046, .T. ) ;
#7812 = DIRECTION ( 'NONE',  ( 0.000000000000000000, 0.000000000000000000, 1.000000000000000000 ) ) ;
#7813 = CYLINDRICAL_SURFACE ( 'NONE', #1364, 1.999999999999971356 ) ;
#7814 = FACE_OUTER_BOUND ( 'NONE', #2610, .T. ) ;
#7815 = CARTESIAN_POINT ( 'NONE',  ( -27.98076211353308551, 52.64999999999986358, -5.000000000000103029 ) ) ;
#7816 = LINE ( 'NONE', #7033, #7836 ) ;
#7817 = CARTESIAN_POINT ( 'NONE',  ( -24.35964822603314772, 55.37708333237728198, -5.935950539335252074 ) ) ;
#7818 = PRESENTATION_STYLE_ASSIGNMENT (( #10478 ) ) ;
#7819 = DIRECTION ( 'NONE',  ( 1.000000000000000000, 0.000000000000000000, 6.308085367188384325E-16 ) ) ;
#7820 = DIRECTION ( 'NONE',  ( -0.000000000000000000, 0.000000000000000000, -1.000000000000000000 ) ) ;
#7821 = ORIENTED_EDGE ( 'NONE', *, *, #4917, .T. ) ;
#7822 = CARTESIAN_POINT ( 'NONE',  ( 1.720978244806812496, 28.18544433887406342, 15.43530841526694175 ) ) ;
#7823 = DIRECTION ( 'NONE',  ( 1.000000000000000000, 6.098637220230963674E-17, 0.000000000000000000 ) ) ;
#7824 = DIRECTION ( 'NONE',  ( 1.000000000000000000, -0.000000000000000000, -0.000000000000000000 ) ) ;
#7825 = CARTESIAN_POINT ( 'NONE',  ( -23.98076211353314235, 55.09999999999986642, -5.000000000000103029 ) ) ;
#7826 = CYLINDRICAL_SURFACE ( 'NONE', #389, 0.4999999999999883982 ) ;
#7827 = CARTESIAN_POINT ( 'NONE',  ( -21.65063509461104374, 12.49999999999986322, 2.500000000000000000 ) ) ;
#7828 = ORIENTED_EDGE ( 'NONE', *, *, #2254, .F. ) ;
#7829 = ADVANCED_FACE ( 'NONE', ( #99 ), #3499, .T. ) ;
#7830 = VERTEX_POINT ( 'NONE', #3327 ) ;
#7831 = CARTESIAN_POINT ( 'NONE',  ( 5.200000000000002842, 0.000000000000000000, 2.500000000000000888 ) ) ;
#7832 = DIRECTION ( 'NONE',  ( 0.000000000000000000, -0.5000000000000012212, -0.8660254037844380415 ) ) ;
#7833 = DIRECTION ( 'NONE',  ( 0.000000000000000000, 0.000000000000000000, 1.000000000000000000 ) ) ;
#7834 = ORIENTED_EDGE ( 'NONE', *, *, #6340, .T. ) ;
#7835 = CARTESIAN_POINT ( 'NONE',  ( 0.000000000000000000, 30.00000000000000000, -2.500000000000000000 ) ) ;
#7836 = VECTOR ( 'NONE', #4372, 1000.000000000000000 ) ;
#7837 = CARTESIAN_POINT ( 'NONE',  ( 0.000000000000000000, -0.8865213383406694847, 1.535500000000001419 ) ) ;
#7838 = ADVANCED_FACE ( 'NONE', ( #1660 ), #9433, .T. ) ;
#7839 = CARTESIAN_POINT ( 'NONE',  ( 20.12303395733248834, 16.58672331782418752, 10.95195673523667246 ) ) ;
#7840 = DIRECTION ( 'NONE',  ( 0.000000000000000000, 0.000000000000000000, 1.000000000000000000 ) ) ;
#7841 = EDGE_CURVE ( 'NONE', #3725, #932, #10197, .T. ) ;
#7842 = CARTESIAN_POINT ( 'NONE',  ( -25.98076211353311393, 53.91874999904394627, -3.128098921329806714 ) ) ;
#7843 = VECTOR ( 'NONE', #1038, 1000.000000000000000 ) ;
#7844 = CARTESIAN_POINT ( 'NONE',  ( -2.649999999999887113, 30.00000000000000000, -2.500000000000000000 ) ) ;
#7845 = VERTEX_POINT ( 'NONE', #8604 ) ;
#7846 = CYLINDRICAL_SURFACE ( 'NONE', #8295, 1.500000000000001332 ) ;
#7847 = VERTEX_POINT ( 'NONE', #159 ) ;
#7848 = CARTESIAN_POINT ( 'NONE',  ( -2.428085025993349078, 27.47833755768751374, 14.37719158473306713 ) ) ;
#7849 = EDGE_LOOP ( 'NONE', ( #5615, #10800, #3902, #5743 ) ) ;
#7850 = CARTESIAN_POINT ( 'NONE',  ( 22.98142095123195716, 18.50759888342988546, 11.95042449705211141 ) ) ;
#7851 = EDGE_CURVE ( 'NONE', #6989, #9904, #3555, .T. ) ;
#7852 = CARTESIAN_POINT ( 'NONE',  ( 24.03139851132786831, 19.63770821034670533, 11.95042449705224996 ) ) ;
#7853 = DIRECTION ( 'NONE',  ( -1.000000000000000000, 0.000000000000000000, 0.000000000000000000 ) ) ;
#7854 = CARTESIAN_POINT ( 'NONE',  ( -27.60187600103308014, 51.52708333237728766, -4.064049460664955760 ) ) ;
#7855 = CARTESIAN_POINT ( 'NONE',  ( 2.649999999999992362, 30.00000000000000000, -2.500000000000000000 ) ) ;
#7856 = VECTOR ( 'NONE', #2042, 1000.000000000000000 ) ;
#7857 = CARTESIAN_POINT ( 'NONE',  ( -2.687328764639638656, 3.067272167851286202, -0.05923475698270370959 ) ) ;
#7858 = DIRECTION ( 'NONE',  ( -0.000000000000000000, 0.000000000000000000, -1.000000000000000000 ) ) ;
#7859 = EDGE_CURVE ( 'NONE', #3727, #4949, #9661, .T. ) ;
#7860 = VERTEX_POINT ( 'NONE', #10499 ) ;
#7861 = EDGE_CURVE ( 'NONE', #10663, #6424, #6103, .T. ) ;
#7862 = EDGE_LOOP ( 'NONE', ( #1885, #10511 ) ) ;
#7863 = CARTESIAN_POINT ( 'NONE',  ( 16.35082997044643704, 18.59891749786092063, 12.19867189564230969 ) ) ;
#7864 = CARTESIAN_POINT ( 'NONE',  ( 25.00000000000000000, 0.000000000000000000, 2.055000000000000160 ) ) ;
#7865 = DIRECTION ( 'NONE',  ( 1.000000000000000000, 6.098637220230963674E-17, 1.156482317317871478E-16 ) ) ;
#7866 = CIRCLE ( 'NONE', #568, 34.99999999999999289 ) ;
#7867 = PLANE ( 'NONE',  #3654 ) ;
#7868 = CARTESIAN_POINT ( 'NONE',  ( 1.274258131564866448, 3.883108878240963513, -3.220599429844046568 ) ) ;
#7869 = CARTESIAN_POINT ( 'NONE',  ( 25.71106610644839208, 56.49999999999984368, 14.50000000000000000 ) ) ;
#7870 = CARTESIAN_POINT ( 'NONE',  ( 2.000000000000000000, 1.773042676681340524, -2.059984127722458425E-15 ) ) ;
#7871 = CARTESIAN_POINT ( 'NONE',  ( 2.474873734152918558, 32.47487373415292211, 14.75000000000000355 ) ) ;
#7872 = CARTESIAN_POINT ( 'NONE',  ( 3.199999999999999734, -3.031088913245509886, 1.750000000000043077 ) ) ;
#7873 = ORIENTED_EDGE ( 'NONE', *, *, #4731, .T. ) ;
#7874 = DIRECTION ( 'NONE',  ( 0.000000000000000000, 0.000000000000000000, 1.000000000000000000 ) ) ;
#7875 = CARTESIAN_POINT ( 'NONE',  ( -0.06616922564517033201, 27.49999999999998934, 15.27905841526694175 ) ) ;
#7876 = CARTESIAN_POINT ( 'NONE',  ( 2.500000000000010214, 28.96446609406726225, 15.76562500000000178 ) ) ;
#7877 = UNCERTAINTY_MEASURE_WITH_UNIT (LENGTH_MEASURE( 1.000000000000000082E-05 ), #7329, 'distance_accuracy_value', 'NONE');
#7878 = EDGE_CURVE ( 'NONE', #1715, #3863, #3632, .T. ) ;
#7879 = DIRECTION ( 'NONE',  ( -0.000000000000000000, -0.000000000000000000, 1.000000000000000000 ) ) ;
#7880 = CARTESIAN_POINT ( 'NONE',  ( 25.00000000000000000, 0.000000000000000000, 2.055000000000000160 ) ) ;
#7881 = CARTESIAN_POINT ( 'NONE',  ( 29.17190429162964094, 2.000000000000001776, -2.500000000000000000 ) ) ;
#7882 = CYLINDRICAL_SURFACE ( 'NONE', #1988, 1.999999999999971356 ) ;
#7883 = VERTEX_POINT ( 'NONE', #1043 ) ;
#7884 = ORIENTED_EDGE ( 'NONE', *, *, #3498, .F. ) ;
#7885 = DIRECTION ( 'NONE',  ( 0.000000000000000000, 0.000000000000000000, -1.000000000000000000 ) ) ;
#7886 = CARTESIAN_POINT ( 'NONE',  ( 4.000000000000000000, 0.000000000000000000, 0.000000000000000000 ) ) ;
#7887 = APPLICATION_PROTOCOL_DEFINITION ( 'draft international standard', 'automotive_design', 1998, #10409 ) ;
#7888 = ORIENTED_EDGE ( 'NONE', *, *, #1594, .F. ) ;
#7889 = AXIS2_PLACEMENT_3D ( 'NONE', #10657, #7208, #8255 ) ;
#7890 = CARTESIAN_POINT ( 'NONE',  ( -6.259644161404860030E-16, -4.618802153517027165, -3.433295621305388234 ) ) ;
#7891 = CARTESIAN_POINT ( 'NONE',  ( 0.000000000000000000, -0.8865213383406730374, -1.535499999999999421 ) ) ;
#7892 = CARTESIAN_POINT ( 'NONE',  ( 22.84119893477061680, 19.75612935582806529, 11.00732503135576401 ) ) ;
#7893 = VECTOR ( 'NONE', #5991, 1000.000000000000000 ) ;
#7894 = CARTESIAN_POINT ( 'NONE',  ( 0.000000000000000000, 0.000000000000000000, 3.499999999999999556 ) ) ;
#7895 = CARTESIAN_POINT ( 'NONE',  ( -27.60187600103308014, 54.38541666571060773, -5.935950539335252074 ) ) ;
#7896 = DIRECTION ( 'NONE',  ( 0.000000000000000000, -1.000000000000000000, 1.471414886128461471E-15 ) ) ;
#7897 = ORIENTED_EDGE ( 'NONE', *, *, #7917, .F. ) ;
#7898 = CARTESIAN_POINT ( 'NONE',  ( 2.500000000000000000, -1.178949249685213863, 2.042000000000002924 ) ) ;
#7899 = ORIENTED_EDGE ( 'NONE', *, *, #9131, .T. ) ;
#7900 = CARTESIAN_POINT ( 'NONE',  ( -2.527408190673963162, 30.96936468028755840, 15.39281658473306358 ) ) ;
#7901 = PRESENTATION_LAYER_ASSIGNMENT (  '', '', ( #1681 ) ) ;
#7902 = EDGE_LOOP ( 'NONE', ( #8943, #1891, #5050, #2066 ) ) ;
#7903 = VECTOR ( 'NONE', #6912, 1000.000000000000000 ) ;
#7904 = CARTESIAN_POINT ( 'NONE',  ( 17.02848097699435215, 16.52496068989110967, 12.06979569234921890 ) ) ;
#7905 = SURFACE_STYLE_FILL_AREA ( #8947 ) ;
#7906 = AXIS2_PLACEMENT_3D ( 'NONE', #8478, #4437, #7819 ) ;
#7907 = CARTESIAN_POINT ( 'NONE',  ( 23.79237391907785693, 22.55645663433636017, 11.95042449705224819 ) ) ;
#7908 = CARTESIAN_POINT ( 'NONE',  ( 20.12931512496741249, 22.03068688373604900, 13.00425721518366728 ) ) ;
#7909 = CARTESIAN_POINT ( 'NONE',  ( -24.35964822603314417, 55.31874999904395196, -5.000000000000103029 ) ) ;
#7910 = AXIS2_PLACEMENT_3D ( 'NONE', #8274, #3218, #9745 ) ;
#7911 = AXIS2_PLACEMENT_3D ( 'NONE', #181, #6791, #3578 ) ;
#7912 = CARTESIAN_POINT ( 'NONE',  ( -4.000000000000000000, 2.309401076758498483, -3.433295621305379353 ) ) ;
#7913 = AXIS2_PLACEMENT_3D ( 'NONE', #4266, #10098, #10039 ) ;
#7914 = FACE_OUTER_BOUND ( 'NONE', #3644, .T. ) ;
#7915 = FACE_OUTER_BOUND ( 'NONE', #4612, .T. ) ;
#7916 = ORIENTED_EDGE ( 'NONE', *, *, #3348, .F. ) ;
#7917 = EDGE_CURVE ( 'NONE', #1487, #10667, #4353, .T. ) ;
#7918 = EDGE_CURVE ( 'NONE', #5275, #7380, #4558, .T. ) ;
#7919 = CARTESIAN_POINT ( 'NONE',  ( 17.59356678224322934, 17.35619608210146581, 12.08212522340233264 ) ) ;
#7920 = VECTOR ( 'NONE', #7523, 1000.000000000000000 ) ;
#7921 = CARTESIAN_POINT ( 'NONE',  ( 3.199999999999987743, 3.375361811986532068, 1.153701847711613215 ) ) ;
#7922 = SURFACE_STYLE_FILL_AREA ( #5474 ) ;
#7923 = AXIS2_PLACEMENT_3D ( 'NONE', #2422, #3428, #6575 ) ;
#7924 = CARTESIAN_POINT ( 'NONE',  ( 25.00000000000000000, 2.055000000000000160, 0.000000000000000000 ) ) ;
#7925 = FACE_OUTER_BOUND ( 'NONE', #2872, .T. ) ;
#7926 = DIRECTION ( 'NONE',  ( -0.000000000000000000, -0.000000000000000000, -1.000000000000000000 ) ) ;
#7927 = CARTESIAN_POINT ( 'NONE',  ( -2.521662442312483599, 27.57191497400664204, 16.37280841526694175 ) ) ;
#7928 = DIRECTION ( 'NONE',  ( -0.000000000000000000, -0.000000000000000000, -1.000000000000000000 ) ) ;
#7929 = VERTEX_POINT ( 'NONE', #9595 ) ;
#7930 = PLANE ( 'NONE',  #2805 ) ;
#7931 = CARTESIAN_POINT ( 'NONE',  ( -2.472591809326051937, 31.10170313157791000, 14.88843341526694353 ) ) ;
#7932 = CARTESIAN_POINT ( 'NONE',  ( -2.649999999999992362, 30.00000000000000000, -2.500000000000000000 ) ) ;
#7933 = CARTESIAN_POINT ( 'NONE',  ( 18.62184541094303114, 16.98042197548449295, 12.02177981800743112 ) ) ;
#7934 = CARTESIAN_POINT ( 'NONE',  ( -26.77982134005685211, 57.38520624385693480, -6.835996254967358965 ) ) ;
#7935 = CARTESIAN_POINT ( 'NONE',  ( -25.17020516978313083, 54.21041666571061057, -6.403925809002825709 ) ) ;
#7936 = DIRECTION ( 'NONE',  ( 0.000000000000000000, 0.000000000000000000, -1.000000000000000000 ) ) ;
#7937 = CARTESIAN_POINT ( 'NONE',  ( 29.50000000000000711, 2.000000000000001776, 17.50099999999999767 ) ) ;
#7938 = ORIENTED_EDGE ( 'NONE', *, *, #9742, .F. ) ;
#7939 =( GEOMETRIC_REPRESENTATION_CONTEXT ( 3 ) GLOBAL_UNCERTAINTY_ASSIGNED_CONTEXT ( ( #4443 ) ) GLOBAL_UNIT_ASSIGNED_CONTEXT ( ( #9003, #1396, #9727 ) ) REPRESENTATION_CONTEXT ( 'NONE', 'WORKASPACE' ) );
#7940 = ORIENTED_EDGE ( 'NONE', *, *, #9790, .F. ) ;
#7941 = CARTESIAN_POINT ( 'NONE',  ( -27.98076211353308551, 54.80833333333319501, -3.845299461620869330 ) ) ;
#7942 = DIRECTION ( 'NONE',  ( 0.000000000000000000, 0.000000000000000000, 1.000000000000000000 ) ) ;
#7943 = ORIENTED_EDGE ( 'NONE', *, *, #6038, .T. ) ;
#7944 = ADVANCED_FACE ( 'NONE', ( #9548 ), #3717, .F. ) ;
#7945 = CARTESIAN_POINT ( 'NONE',  ( -25.98076211353324894, 16.50000000000026290, -5.000000000000000000 ) ) ;
#7946 = CARTESIAN_POINT ( 'NONE',  ( 0.000000000000000000, 30.00000000000000000, -23.71320343559643007 ) ) ;
#7947 = AXIS2_PLACEMENT_3D ( 'NONE', #3185, #6566, #6738 ) ;
#7948 = AXIS2_PLACEMENT_3D ( 'NONE', #8384, #9218, #5174 ) ;
#7949 = CARTESIAN_POINT ( 'NONE',  ( 16.85117638942448082, 18.09857107888056760, 11.14955153432450530 ) ) ;
#7950 = ORIENTED_EDGE ( 'NONE', *, *, #7491, .T. ) ;
#7951 = CARTESIAN_POINT ( 'NONE',  ( -25.17020516978313083, 51.87708333237728198, -3.596074190997380349 ) ) ;
#7952 = VERTEX_POINT ( 'NONE', #2111 ) ;
#7953 = FACE_OUTER_BOUND ( 'NONE', #563, .T. ) ;
#7954 = ORIENTED_EDGE ( 'NONE', *, *, #4130, .T. ) ;
#7955 = AXIS2_PLACEMENT_3D ( 'NONE', #1405, #10677, #4115 ) ;
#7956 = CARTESIAN_POINT ( 'NONE',  ( 1.035533905932737975, 32.50000000000000711, 13.57812500000000178 ) ) ;
#7957 = VERTEX_POINT ( 'NONE', #320 ) ;
#7958 = CARTESIAN_POINT ( 'NONE',  ( 18.60991190964745456, 16.01828113007465504, 10.97873183052796620 ) ) ;
#7959 = DIRECTION ( 'NONE',  ( -0.7055570967602537991, 0.7055570967602550203, 0.06616922564517474514 ) ) ;
#7960 = MECHANICAL_DESIGN_GEOMETRIC_PRESENTATION_REPRESENTATION (  '', ( #10265 ), #7600 ) ;
#7961 = CARTESIAN_POINT ( 'NONE',  ( 16.77403034288735029, 16.76147925670542094, 13.09486341078152805 ) ) ;
#7962 = CARTESIAN_POINT ( 'NONE',  ( -26.79131905728310059, 54.15208333237728056, -6.403925809002825709 ) ) ;
#7963 = AXIS2_PLACEMENT_3D ( 'NONE', #7529, #2532, #860 ) ;
#7964 = DIRECTION ( 'NONE',  ( 0.8660254037844398178, -0.4999999999999978351, 0.000000000000000000 ) ) ;
#7965 = DIRECTION ( 'NONE',  ( -0.000000000000000000, 1.000000000000000000, -0.000000000000000000 ) ) ;
#7966 = CARTESIAN_POINT ( 'NONE',  ( -24.98076211353312814, 53.02916666475469754, -6.732050807568954909 ) ) ;
#7967 = EDGE_CURVE ( 'NONE', #6486, #4305, #1949, .T. ) ;
#7968 = ORIENTED_EDGE ( 'NONE', *, *, #1250, .T. ) ;
#7969 = ORIENTED_EDGE ( 'NONE', *, *, #3177, .F. ) ;
#7970 = CARTESIAN_POINT ( 'NONE',  ( 29.49999999999999645, 1.387778780781445676E-14, -12.49999999999999822 ) ) ;
#7971 = FACE_OUTER_BOUND ( 'NONE', #958, .T. ) ;
#7972 = CARTESIAN_POINT ( 'NONE',  ( 0.000000000000000000, -3.031088913245550298, -1.749999999999972911 ) ) ;
#7973 = CYLINDRICAL_SURFACE ( 'NONE', #9325, 24.99999999999999645 ) ;
#7974 = CARTESIAN_POINT ( 'NONE',  ( -26.51666049839534267, 55.91876073720499818, -7.000000000000075495 ) ) ;
#7975 = SHAPE_REPRESENTATION ( 'domed cap nut_din_DIN 1587 - M4 --NNU', ( #308 ), #8995 ) ;
#7976 = CARTESIAN_POINT ( 'NONE',  ( 0.3126073911696528040, 2.020725942163738686, 3.499999999999999556 ) ) ;
#7977 = EDGE_CURVE ( 'NONE', #2292, #491, #5331, .T. ) ;
#7978 = FACE_OUTER_BOUND ( 'NONE', #690, .T. ) ;
#7979 = CARTESIAN_POINT ( 'NONE',  ( 1.383578242660657098, 33.52740819067396671, 12.58031658473306713 ) ) ;
#7980 = FACE_BOUND ( 'NONE', #7862, .T. ) ;
#7981 = ORIENTED_EDGE ( 'NONE', *, *, #5542, .T. ) ;
#7982 = SURFACE_SIDE_STYLE ('',( #6246 ) ) ;
#7983 = EDGE_CURVE ( 'NONE', #2134, #6926, #7105, .T. ) ;
#7984 = CARTESIAN_POINT ( 'NONE',  ( 0.9693646802875698354, 27.47259180932603684, 16.60718341526694175 ) ) ;
#7985 = CARTESIAN_POINT ( 'NONE',  ( -1.035533905932736420, 27.49999999999998934, 15.45312500000000178 ) ) ;
#7986 = CARTESIAN_POINT ( 'NONE',  ( 23.13231036272843966, 20.08340223762181154, 12.00579112326941988 ) ) ;
#7987 = CARTESIAN_POINT ( 'NONE',  ( -25.44486372867087809, 55.15623925897106261, -7.000000000000075495 ) ) ;
#7988 = LINE ( 'NONE', #6252, #4880 ) ;
#7989 = ADVANCED_FACE ( 'NONE', ( #8766 ), #8830, .T. ) ;
#7990 = CARTESIAN_POINT ( 'NONE',  ( 11.61000000000001542, 0.000000000000000000, 0.000000000000000000 ) ) ;
#7991 = CARTESIAN_POINT ( 'NONE',  ( -26.79131905728310059, 50.82708333237727771, -6.403925809002825709 ) ) ;
#7992 = DIRECTION ( 'NONE',  ( -1.000000000000000000, -6.098637220230964906E-17, -6.308085367188384325E-16 ) ) ;
#7993 = DIRECTION ( 'NONE',  ( 0.000000000000000000, 0.000000000000000000, 1.000000000000000000 ) ) ;
#7994 = EDGE_LOOP ( 'NONE', ( #3056, #9559, #7165, #10768, #6761, #9669, #3342, #3768, #4178, #6711, #404, #6285, #8166, #9147 ) ) ;
#7995 = VERTEX_POINT ( 'NONE', #1095 ) ;
#7996 = CARTESIAN_POINT ( 'NONE',  ( -25.44486372867087454, 50.66876073720499818, -3.000000000000134559 ) ) ;
#7997 = ADVANCED_FACE ( 'NONE', ( #9653 ), #4614, .T. ) ;
#7998 = EDGE_CURVE ( 'NONE', #3058, #170, #5500, .T. ) ;
#7999 = CARTESIAN_POINT ( 'NONE',  ( 4.800000000000000711, 0.000000000000000000, 0.000000000000000000 ) ) ;
#8000 = CONTEXT_DEPENDENT_SHAPE_REPRESENTATION ( #8101, #923 ) ;
#8001 = ORIENTED_EDGE ( 'NONE', *, *, #4731, .F. ) ;
#8002 = CYLINDRICAL_SURFACE ( 'NONE', #1329, 2.149999999999990585 ) ;
#8003 = CARTESIAN_POINT ( 'NONE',  ( -26.79131905728310059, 50.88541666571061484, -3.596074190997381237 ) ) ;
#8004 = CARTESIAN_POINT ( 'NONE',  ( 22.60530603367148927, 19.52972610220585636, 11.00732503135576401 ) ) ;
#8005 = EDGE_LOOP ( 'NONE', ( #6098, #7873, #10601, #4292 ) ) ;
#8006 = CARTESIAN_POINT ( 'NONE',  ( -25.17020516978313083, 53.51041666571060773, -6.403925809002825709 ) ) ;
#8007 = ORIENTED_EDGE ( 'NONE', *, *, #8785, .T. ) ;
#8008 = DIRECTION ( 'NONE',  ( -1.000000000000000000, -0.000000000000000000, -0.000000000000000000 ) ) ;
#8009 = ORIENTED_EDGE ( 'NONE', *, *, #6466, .F. ) ;
#8010 = CARTESIAN_POINT ( 'NONE',  ( -1.767766952966375094, 31.76776695296636888, 13.81250000000000355 ) ) ;
#8011 = ORIENTED_EDGE ( 'NONE', *, *, #4667, .F. ) ;
#8012 = CARTESIAN_POINT ( 'NONE',  ( 20.12303395733248834, 16.58672331782418752, 10.95195673523667246 ) ) ;
#8013 = ADVANCED_FACE ( 'NONE', ( #263 ), #3661, .T. ) ;
#8014 = CARTESIAN_POINT ( 'NONE',  ( 4.211140560182196957, 2.431303136016536470, -3.745885042887433514 ) ) ;
#8015 = CARTESIAN_POINT ( 'NONE',  ( 17.64011212484924940, 17.30965061758477219, 13.07995645546588825 ) ) ;
#8016 = CARTESIAN_POINT ( 'NONE',  ( -23.98076211353314235, 49.55833333333319501, -6.154700538379337615 ) ) ;
#8017 = AXIS2_PLACEMENT_3D ( 'NONE', #2297, #5688, #8227 ) ;
#8018 = FACE_OUTER_BOUND ( 'NONE', #8703, .T. ) ;
#8019 = CARTESIAN_POINT ( 'NONE',  ( 29.50000000000000711, 1.387778780781445676E-14, -12.50000000000000000 ) ) ;
#8020 = EDGE_LOOP ( 'NONE', ( #10188, #3347, #6024, #2442, #2063 ) ) ;
#8021 = ORIENTED_EDGE ( 'NONE', *, *, #3905, .T. ) ;
#8022 = CARTESIAN_POINT ( 'NONE',  ( 19.77604874367146692, 21.01153129092389094, 12.00579112326941988 ) ) ;
#8023 = DIRECTION ( 'NONE',  ( -1.000000000000000000, 0.000000000000000000, 0.000000000000000000 ) ) ;
#8024 = ADVANCED_FACE ( 'NONE', ( #25 ), #7760, .T. ) ;
#8025 = CARTESIAN_POINT ( 'NONE',  ( 34.99999999999999289, -2.999999999999977796, -17.49999999999999645 ) ) ;
#8026 = CIRCLE ( 'NONE', #2345, 1.535500000000000087 ) ;
#8027 = DIRECTION ( 'NONE',  ( 0.000000000000000000, 0.000000000000000000, 1.000000000000000000 ) ) ;
#8028 = PRESENTATION_STYLE_ASSIGNMENT (( #5365 ) ) ;
#8029 = CARTESIAN_POINT ( 'NONE',  ( -1.449747468305830678, 26.49999999999999289, 14.20312500000000355 ) ) ;
#8030 = FACE_BOUND ( 'NONE', #9451, .T. ) ;
#8031 = ORIENTED_EDGE ( 'NONE', *, *, #4506, .F. ) ;
#8032 = DIRECTION ( 'NONE',  ( -1.000000000000000000, -6.098637220230963674E-17, -1.156482317317871725E-16 ) ) ;
#8033 = CARTESIAN_POINT ( 'NONE',  ( 2.428085025993357071, 27.47833755768751374, 16.68530841526694175 ) ) ;
#8034 = CARTESIAN_POINT ( 'NONE',  ( -2.500000000000007550, 30.06616922564517580, 14.96655841526694175 ) ) ;
#8035 = VECTOR ( 'NONE', #7261, 1000.000000000000114 ) ;
#8036 = CARTESIAN_POINT ( 'NONE',  ( 19.13264607096459002, 17.09257730534942965, 12.00833071292064425 ) ) ;
#8037 = CARTESIAN_POINT ( 'NONE',  ( 0.000000000000000000, -1.178949249685218303, -2.041999999999998039 ) ) ;
#8038 = DIRECTION ( 'NONE',  ( 0.000000000000000000, 0.000000000000000000, 1.000000000000000000 ) ) ;
#8039 = CARTESIAN_POINT ( 'NONE',  ( -23.98076211353314235, 51.65833333333319644, -6.154700538379337615 ) ) ;
#8040 = CARTESIAN_POINT ( 'NONE',  ( -27.60187600103308014, 51.00208333237728198, -4.064049460664955760 ) ) ;
#8041 = CARTESIAN_POINT ( 'NONE',  ( 29.49999999999999289, 6.938893903907228378E-15, 17.50000000000000000 ) ) ;
#8042 = LINE ( 'NONE', #6524, #10398 ) ;
#8043 = VERTEX_POINT ( 'NONE', #2760 ) ;
#8044 = CARTESIAN_POINT ( 'NONE',  ( 34.99999999999987210, -2.999999999999962252, -17.49999999999999645 ) ) ;
#8045 = EDGE_CURVE ( 'NONE', #1687, #7662, #10914, .T. ) ;
#8046 = EDGE_LOOP ( 'NONE', ( #2322, #4101, #8956, #7138 ) ) ;
#8047 = EDGE_CURVE ( 'NONE', #3381, #6762, #3484, .T. ) ;
#8048 = DIRECTION ( 'NONE',  ( 0.000000000000000000, 0.000000000000000000, -1.000000000000000000 ) ) ;
#8049 = CARTESIAN_POINT ( 'NONE',  ( 19.92593468680574986, 17.66592327340909918, 11.00732503135576401 ) ) ;
#8050 = ORIENTED_EDGE ( 'NONE', *, *, #3317, .F. ) ;
#8051 = CARTESIAN_POINT ( 'NONE',  ( 0.000000000000000000, 0.000000000000000000, -2.500000000000000000 ) ) ;
#8052 = ORIENTED_EDGE ( 'NONE', *, *, #9101, .T. ) ;
#8053 = CARTESIAN_POINT ( 'NONE',  ( 4.750000000000000888, -1.622657008870242882E-15, 0.000000000000000000 ) ) ;
#8054 = ORIENTED_EDGE ( 'NONE', *, *, #5808, .F. ) ;
#8055 = CARTESIAN_POINT ( 'NONE',  ( -2.500000000000003997, 29.93383077435482065, 15.47094158473306535 ) ) ;
#8056 = ORIENTED_EDGE ( 'NONE', *, *, #10578, .T. ) ;
#8057 = CARTESIAN_POINT ( 'NONE',  ( 23.98154255942039370, 19.66242269470938453, 10.95195840513859586 ) ) ;
#8058 = SURFACE_STYLE_USAGE ( .BOTH. , #4740 ) ;
#8059 = AXIS2_PLACEMENT_3D ( 'NONE', #6632, #10203, #5158 ) ;
#8060 = FACE_OUTER_BOUND ( 'NONE', #3676, .T. ) ;
#8061 = CARTESIAN_POINT ( 'NONE',  ( 17.91214753276079819, 17.12229137291643610, 13.05912755560225236 ) ) ;
#8062 = CARTESIAN_POINT ( 'NONE',  ( -3.456897879362374582, 29.45240795142739998, 16.49922112211940117 ) ) ;
#8063 = VECTOR ( 'NONE', #7824, 1000.000000000000000 ) ;
#8064 = DIRECTION ( 'NONE',  ( -1.000000000000000000, -0.000000000000000000, -0.000000000000000000 ) ) ;
#8065 = DIRECTION ( 'NONE',  ( -1.000000000000000000, -0.000000000000000000, -0.000000000000000000 ) ) ;
#8066 = EDGE_LOOP ( 'NONE', ( #2077, #10852, #10065, #5931, #551 ) ) ;
#8067 = CIRCLE ( 'NONE', #10565, 35.00000000000000000 ) ;
#8068 = VECTOR ( 'NONE', #10547, 1000.000000000000000 ) ;
#8069 = EDGE_LOOP ( 'NONE', ( #9419, #8588, #6432, #6257 ) ) ;
#8070 = CARTESIAN_POINT ( 'NONE',  ( 17.25670323398246353, 17.69304423432567930, 13.11591282735340336 ) ) ;
#8071 = ADVANCED_FACE ( 'NONE', ( #9366 ), #190, .T. ) ;
#8072 = DIRECTION ( 'NONE',  ( 1.000000000000000000, 0.000000000000000000, 0.000000000000000000 ) ) ;
#8073 = VECTOR ( 'NONE', #3334, 1000.000000000000114 ) ;
#8074 = CARTESIAN_POINT ( 'NONE',  ( 25.49999999999999645, -3.999999999999983569, 8.350000000000010303 ) ) ;
#8075 = CIRCLE ( 'NONE', #10911, 2.149999999999992362 ) ;
#8076 = CARTESIAN_POINT ( 'NONE',  ( -27.98076211353308551, 56.06249999808802897, -5.000000000000103029 ) ) ;
#8078 = DIRECTION ( 'NONE',  ( 0.000000000000000000, 0.000000000000000000, -1.000000000000000000 ) ) ;
#8077 = AXIS2_PLACEMENT_3D ( 'NONE', #4367, #2414, #5798 ) ;
#8079 = AXIS2_PLACEMENT_3D ( 'NONE', #5334, #1997, #8048 ) ;
#8080 = CYLINDRICAL_SURFACE ( 'NONE', #4431, 5.000000000000000888 ) ;
#8081 = CARTESIAN_POINT ( 'NONE',  ( -2.474873734152920335, 32.47487373415291501, 16.31250000000000355 ) ) ;
#8082 = FACE_OUTER_BOUND ( 'NONE', #6603, .T. ) ;
#8083 = UNCERTAINTY_MEASURE_WITH_UNIT (LENGTH_MEASURE( 1.000000000000000082E-05 ), #4537, 'distance_accuracy_value', 'NONE');
#8084 = ORIENTED_EDGE ( 'NONE', *, *, #6200, .F. ) ;
#8085 = DIRECTION ( 'NONE',  ( -6.098637220230963674E-17, 1.000000000000000000, 0.000000000000000000 ) ) ;
#8086 = VECTOR ( 'NONE', #8864, 1000.000000000000114 ) ;
#8087 =( BOUNDED_CURVE ( )  B_SPLINE_CURVE ( 2, ( #6601, #4747, #6397, #4002, #4963, #3900, #10722, #9163, #3120 ),
 .UNSPECIFIED., .F., .F. ) 
 B_SPLINE_CURVE_WITH_KNOTS ( ( 3, 2, 2, 2, 3 ),
 ( 0.5833333333333333703, 0.5925925925925925597, 0.6111111111111111605, 0.6296296296296296502, 0.6388888888888889506 ),
 .UNSPECIFIED. ) 
 CURVE ( )  GEOMETRIC_REPRESENTATION_ITEM ( )  RATIONAL_B_SPLINE_CURVE ( ( 0.9330127018922194093, 0.9330127018922197424, 1.000000000000000000, 0.8660254037844387076, 1.000000000000000000, 0.8660254037844387076, 1.000000000000000000, 0.9330127018922189652, 0.9330127018922194093 ) ) 
 REPRESENTATION_ITEM ( '' )  );
#8088 = CARTESIAN_POINT ( 'NONE',  ( 2.521662442312485819, 32.42808502599335441, 14.49780841526694175 ) ) ;
#8089 = VECTOR ( 'NONE', #1765, 1000.000000000000000 ) ;
#8090 = LINE ( 'NONE', #3037, #7384 ) ;
#8091 = CARTESIAN_POINT ( 'NONE',  ( 2.000000000000000000, -0.8865213383406730374, -1.535499999999999421 ) ) ;
#8092 = LINE ( 'NONE', #1201, #10563 ) ;
#8093 = CARTESIAN_POINT ( 'NONE',  ( -24.35964822603314772, 53.33541666571061057, -4.064049460664953983 ) ) ;
#8094 = CARTESIAN_POINT ( 'NONE',  ( 2.982310868302101792, -1.691919446221600731, 3.499999999999999556 ) ) ;
#8095 = CARTESIAN_POINT ( 'NONE',  ( -2.836893136758495970, -3.208949435745868328, -3.505054077164885484 ) ) ;
#8096 = AXIS2_PLACEMENT_3D ( 'NONE', #10470, #2864, #8636 ) ;
#8097 = VERTEX_POINT ( 'NONE', #913 ) ;
#8098 = DIRECTION ( 'NONE',  ( -0.000000000000000000, 1.000000000000000000, -0.000000000000000000 ) ) ;
#8099 = DIRECTION ( 'NONE',  ( -1.000000000000000000, -0.000000000000000000, -0.000000000000000000 ) ) ;
#8100 = ORIENTED_EDGE ( 'NONE', *, *, #4180, .T. ) ;
#8101 =( REPRESENTATION_RELATIONSHIP ('NONE','NONE', #7540, #5757 ) REPRESENTATION_RELATIONSHIP_WITH_TRANSFORMATION ( #8154 )SHAPE_REPRESENTATION_RELATIONSHIP( ) );
#8102 = CARTESIAN_POINT ( 'NONE',  ( 0.000000000000000000, 0.000000000000000000, 2.500000000000000000 ) ) ;
#8103 = CIRCLE ( 'NONE', #2251, 1.649999999999989919 ) ;
#8104 = CARTESIAN_POINT ( 'NONE',  ( -25.17020516978313083, 51.23541666571061626, -6.403925809002825709 ) ) ;
#8105 = CARTESIAN_POINT ( 'NONE',  ( 21.22493709936120254, 18.56951933379358621, 11.00732503135576401 ) ) ;
#8106 = VERTEX_POINT ( 'NONE', #6923 ) ;
#8107 = EDGE_CURVE ( 'NONE', #6726, #2763, #439, .T. ) ;
#8108 = CARTESIAN_POINT ( 'NONE',  ( -27.44132740410865523, 55.89336612041926600, -4.296608737464627126 ) ) ;
#8109 = ORIENTED_EDGE ( 'NONE', *, *, #3959, .T. ) ;
#8110 = DIRECTION ( 'NONE',  ( 0.000000000000000000, 0.000000000000000000, 1.000000000000000000 ) ) ;
#8111 = ORIENTED_EDGE ( 'NONE', *, *, #2396, .T. ) ;
#8112 = EDGE_CURVE ( 'NONE', #10495, #9728, #7705, .T. ) ;
#8113 = CARTESIAN_POINT ( 'NONE',  ( -1.101703131577916883, 32.47259180932605460, 13.98656658473306713 ) ) ;
#8114 = ORIENTED_EDGE ( 'NONE', *, *, #8045, .F. ) ;
#8116 = CARTESIAN_POINT ( 'NONE',  ( 23.50695973324029353, 19.00259546466308791, 10.95195840513859231 ) ) ;
#8115 = CIRCLE ( 'NONE', #4754, 4.000000000000000000 ) ;
#8117 = PRODUCT_DEFINITION_FORMATION_WITH_SPECIFIED_SOURCE ( 'ANY', '', #218, .NOT_KNOWN. ) ;
#8118 = CYLINDRICAL_SURFACE ( 'NONE', #4033, 4.499999999999999112 ) ;
#8119 = CARTESIAN_POINT ( 'NONE',  ( 23.39622245855813176, 20.94697541805627239, 13.00425721518248956 ) ) ;
#8120 = EDGE_CURVE ( 'NONE', #12, #4811, #933, .T. ) ;
#8121 = CARTESIAN_POINT ( 'NONE',  ( -26.98076211353309972, 51.04583333142137036, -6.732050807568954909 ) ) ;
#8122 = AXIS2_PLACEMENT_3D ( 'NONE', #9015, #6108, #7623 ) ;
#8123 = AXIS2_PLACEMENT_3D ( 'NONE', #3623, #3733, #6339 ) ;
#8124 = CARTESIAN_POINT ( 'NONE',  ( 34.66939463810009414, 4.803388076618548830, -2.500000000000000444 ) ) ;
#8125 = B_SPLINE_CURVE_WITH_KNOTS ( 'NONE', 3,
 ( #10383, #8669, #5996, #991, #7614, #3558 ),
 .UNSPECIFIED., .F., .F.,
 ( 4, 2, 4 ),
 ( 0.002044882221487493313, 0.003063384235218477233, 0.004081886248949461587 ),
 .UNSPECIFIED. ) ;
#8126 = VERTEX_POINT ( 'NONE', #861 ) ;
#8127 = ORIENTED_EDGE ( 'NONE', *, *, #1393, .F. ) ;
#8128 = ADVANCED_FACE ( 'NONE', ( #10363 ), #3287, .T. ) ;
#8129 = CARTESIAN_POINT ( 'NONE',  ( 20.73695268571362504, 18.16262921024512167, 12.00579112326941988 ) ) ;
#8130 = AXIS2_PLACEMENT_3D ( 'NONE', #180, #6911, #5141 ) ;
#8131 = CARTESIAN_POINT ( 'NONE',  ( 21.21106610644839208, 53.49999999999983658, 10.00000000000000178 ) ) ;
#8132 = DIRECTION ( 'NONE',  ( 0.000000000000000000, 0.000000000000000000, 1.000000000000000000 ) ) ;
#8133 = DIRECTION ( 'NONE',  ( 1.000000000000000000, -0.000000000000000000, 1.156482317317871478E-16 ) ) ;
#8134 = APPLICATION_CONTEXT ( 'automotive_design' ) ;
#8135 = DIRECTION ( 'NONE',  ( -1.000000000000000000, 0.000000000000000000, 0.000000000000000000 ) ) ;
#8136 = CARTESIAN_POINT ( 'NONE',  ( 2.521662442312487151, 27.57191497400665270, 14.68969158473306535 ) ) ;
#8137 = PLANE ( 'NONE',  #4561 ) ;
#8138 = EDGE_CURVE ( 'NONE', #8106, #7431, #3470, .T. ) ;
#8139 = ORIENTED_EDGE ( 'NONE', *, *, #7038, .T. ) ;
#8140 =( NAMED_UNIT ( * ) SI_UNIT ( $, .STERADIAN. ) SOLID_ANGLE_UNIT ( ) );
#8141 = AXIS2_PLACEMENT_3D ( 'NONE', #5639, #10116, #2503 ) ;
#8142 = CARTESIAN_POINT ( 'NONE',  ( -3.472591809326048384, 31.51591669395100936, 16.13843341526694530 ) ) ;
#8143 = CARTESIAN_POINT ( 'NONE',  ( -4.204114297095464359, 1.660363174096617156, -3.602136431857887011 ) ) ;
#8144 = CARTESIAN_POINT ( 'NONE',  ( 0.000000000000000000, 0.000000000000000000, 0.000000000000000000 ) ) ;
#8145 = B_SPLINE_CURVE_WITH_KNOTS ( 'NONE', 3,
 ( #4475, #7079, #10520, #3847, #7857, #4580, #1176, #1293 ),
 .UNSPECIFIED., .F., .F.,
 ( 4, 2, 2, 4 ),
 ( 2.465131517071352357E-07, 0.001183067374689843057, 0.001774477805458910071, 0.002365888236227977302 ),
 .UNSPECIFIED. ) ;
#8146 = CARTESIAN_POINT ( 'NONE',  ( -1.767766952966375094, 31.76776695296636888, 13.81250000000000355 ) ) ;
#8147 = CARTESIAN_POINT ( 'NONE',  ( -24.98076211353313170, 51.48333333333319928, -3.267949192431250705 ) ) ;
#8148 = CARTESIAN_POINT ( 'NONE',  ( -27.60187600103308370, 50.94374999904394485, -5.000000000000103029 ) ) ;
#8149 = DIRECTION ( 'NONE',  ( -1.000000000000000000, -0.000000000000000000, -0.000000000000000000 ) ) ;
#8150 = FACE_OUTER_BOUND ( 'NONE', #5694, .T. ) ;
#8151 = ORIENTED_EDGE ( 'NONE', *, *, #5387, .T. ) ;
#8152 = LINE ( 'NONE', #10337, #8035 ) ;
#8153 = CARTESIAN_POINT ( 'NONE',  ( -25.98076211353311393, 59.49999999999985789, -5.000000000000103029 ) ) ;
#8154 = ITEM_DEFINED_TRANSFORMATION ( 'NONE', 'NONE', #5457,  #308 ) ;
#8155 = ORIENTED_EDGE ( 'NONE', *, *, #5502, .F. ) ;
#8156 = PLANE ( 'NONE',  #7012 ) ;
#8157 = CARTESIAN_POINT ( 'NONE',  ( -25.17020516978313083, 51.93541666571061910, -6.403925809002825709 ) ) ;
#8158 = ADVANCED_FACE ( 'NONE', ( #8586 ), #1866, .F. ) ;
#8159 = CARTESIAN_POINT ( 'NONE',  ( 19.13264607096459002, 17.09257730534942965, 12.00833071292064425 ) ) ;
#8160 = VERTEX_POINT ( 'NONE', #3369 ) ;
#8161 = CARTESIAN_POINT ( 'NONE',  ( -27.98076211353308551, 53.90416666475469754, -6.154700538379338504 ) ) ;
#8162 = VERTEX_POINT ( 'NONE', #8536 ) ;
#8163 = CARTESIAN_POINT ( 'NONE',  ( -27.44132332507749794, 55.71836679508493262, -4.296600267573891685 ) ) ;
#8164 = ORIENTED_EDGE ( 'NONE', *, *, #2089, .T. ) ;
#8165 = DIRECTION ( 'NONE',  ( -1.000000000000000000, -0.000000000000000000, -0.000000000000000000 ) ) ;
#8166 = ORIENTED_EDGE ( 'NONE', *, *, #8514, .T. ) ;
#8167 = CARTESIAN_POINT ( 'NONE',  ( 19.72987285752124720, 16.32873191470754648, 10.95281372472358861 ) ) ;
#8168 = EDGE_CURVE ( 'NONE', #10992, #8562, #10492, .T. ) ;
#8169 = CARTESIAN_POINT ( 'NONE',  ( 3.455068668934414777, -2.624017327439094327, -3.316620875263732504 ) ) ;
#8170 = ADVANCED_FACE ( 'NONE', ( #9302 ), #5097, .T. ) ;
#8171 = CARTESIAN_POINT ( 'NONE',  ( 15.40853749019034069, 18.12699641572163145, 12.22072830420661660 ) ) ;
#8172 = CARTESIAN_POINT ( 'NONE',  ( -25.98076211353311393, 50.28749999808803040, -7.309401076758571314 ) ) ;
#8173 = LINE ( 'NONE', #1560, #5600 ) ;
#8174 = CARTESIAN_POINT ( 'NONE',  ( -25.98076211353311393, 50.98749999808804034, -7.000000000000073719 ) ) ;
#8175 = ORIENTED_EDGE ( 'NONE', *, *, #573, .T. ) ;
#8176 = ORIENTED_EDGE ( 'NONE', *, *, #4585, .T. ) ;
#8177 = CARTESIAN_POINT ( 'NONE',  ( 19.84380896203909828, 21.37294244821887546, 12.00579112326902731 ) ) ;
#8178 = ADVANCED_FACE ( 'NONE', ( #10199 ), #6977, .T. ) ;
#8179 = EDGE_CURVE ( 'NONE', #12, #10561, #1090, .T. ) ;
#8180 = AXIS2_PLACEMENT_3D ( 'NONE', #4072, #723, #7511 ) ;
#8181 = CARTESIAN_POINT ( 'NONE',  ( 0.3126073911696294338, 2.020725942163657862, -3.499999999999999556 ) ) ;
#8182 = CARTESIAN_POINT ( 'NONE',  ( 5.200000000000002842, 3.061616997868384127E-16, -2.500000000000000888 ) ) ;
#8183 = LINE ( 'NONE', #3181, #27 ) ;
#8184 = DIRECTION ( 'NONE',  ( 1.000000000000000000, 0.000000000000000000, 0.000000000000000000 ) ) ;
#8185 = CARTESIAN_POINT ( 'NONE',  ( 1.101703131577918438, 27.52740819067395606, 13.36156658473306535 ) ) ;
#8186 = LINE ( 'NONE', #7193, #7031 ) ;
#8187 = ORIENTED_EDGE ( 'NONE', *, *, #7285, .F. ) ;
#8188 = DIRECTION ( 'NONE',  ( 0.000000000000000000, 0.000000000000000000, 1.000000000000000000 ) ) ;
#8189 = ORIENTED_EDGE ( 'NONE', *, *, #10345, .T. ) ;
#8190 = CONICAL_SURFACE ( 'NONE', #2700, 4.624785217660733139, 1.047197551196604071 ) ;
#8191 = CARTESIAN_POINT ( 'NONE',  ( -2.500000000000007550, 30.06616922564517580, 16.21655841526694175 ) ) ;
#8192 = DIRECTION ( 'NONE',  ( 6.098637220230963674E-17, -1.000000000000000000, 0.000000000000000000 ) ) ;
#8193 = DIRECTION ( 'NONE',  ( -1.000000000000000000, 0.000000000000000000, 0.000000000000000000 ) ) ;
#8194 = CARTESIAN_POINT ( 'NONE',  ( -1.767766952966370209, 28.23223304703362402, 14.12500000000000355 ) ) ;
#8195 = CARTESIAN_POINT ( 'NONE',  ( -0.5276280594146446346, 4.314175951381965746, -3.320322319201721495 ) ) ;
#8196 = CARTESIAN_POINT ( 'NONE',  ( -24.35964822603314772, 51.76041666571060773, -4.064049460664953983 ) ) ;
#8197 = CARTESIAN_POINT ( 'NONE',  ( 3.511755186886750923, -2.826662030176382956, -3.597382984111582083 ) ) ;
#8198 = CARTESIAN_POINT ( 'NONE',  ( 0.2500000000000002220, 0.000000000000000000, 4.250000000000000000 ) ) ;
#8199 = ORIENTED_EDGE ( 'NONE', *, *, #10813, .F. ) ;
#8200 = DIRECTION ( 'NONE',  ( -1.000000000000000000, 0.000000000000000000, 0.000000000000000000 ) ) ;
#8201 = AXIS2_PLACEMENT_3D ( 'NONE', #4388, #10323, #7773 ) ;
#8202 = DIRECTION ( 'NONE',  ( -1.000000000000000000, -0.000000000000000000, -0.000000000000000000 ) ) ;
#8203 = CARTESIAN_POINT ( 'NONE',  ( -25.98076211353311038, 59.49999999999985789, -5.000000000000102141 ) ) ;
#8204 = CARTESIAN_POINT ( 'NONE',  ( -26.79131905728310059, 52.98541666571061626, -3.596074190997381237 ) ) ;
#8205 = CARTESIAN_POINT ( 'NONE',  ( 20.47715220320264962, 17.98190999816754498, 12.00579112326941988 ) ) ;
#8206 = CARTESIAN_POINT ( 'NONE',  ( -26.79131905728310059, 55.55208333237728624, -6.403925809002825709 ) ) ;
#8207 = ORIENTED_EDGE ( 'NONE', *, *, #7654, .T. ) ;
#8208 = DIRECTION ( 'NONE',  ( -1.000000000000000000, 0.000000000000000000, 0.000000000000000000 ) ) ;
#8209 = ORIENTED_EDGE ( 'NONE', *, *, #3582, .F. ) ;
#8210 = ORIENTED_EDGE ( 'NONE', *, *, #8514, .F. ) ;
#8211 = CARTESIAN_POINT ( 'NONE',  ( -30.75045812061784289, 13.49999999999941913, -5.000000000000000000 ) ) ;
#8212 = ORIENTED_EDGE ( 'NONE', *, *, #9770, .T. ) ;
#8213 = CARTESIAN_POINT ( 'NONE',  ( 2.500000000000010214, 28.96446609406726225, 15.76562500000000178 ) ) ;
#8214 = ORIENTED_EDGE ( 'NONE', *, *, #10789, .T. ) ;
#8215 = CARTESIAN_POINT ( 'NONE',  ( 22.93505243896877133, 21.90805399618153970, 11.00732503135576401 ) ) ;
#8216 = CARTESIAN_POINT ( 'NONE',  ( -0.1404048886732797152, -4.699864953788083888, -3.686887068327043160 ) ) ;
#8217 = CARTESIAN_POINT ( 'NONE',  ( 19.53332707643461319, 16.11782042516817981, 12.95310296989756260 ) ) ;
#8218 = CARTESIAN_POINT ( 'NONE',  ( -26.98076211353309972, 50.34583333142136752, -6.732050807568954909 ) ) ;
#8219 = CARTESIAN_POINT ( 'NONE',  ( 34.86967549602667304, 3.020777328503462034, -3.237032597732066197 ) ) ;
#8220 = CARTESIAN_POINT ( 'NONE',  ( -25.98076211353311393, 51.33749999808802755, -3.000000000000132783 ) ) ;
#8221 = EDGE_LOOP ( 'NONE', ( #1981, #2172, #9430, #2823 ) ) ;
#8222 = CARTESIAN_POINT ( 'NONE',  ( -3.527408190673961386, 28.61642175733934224, 16.29468341526694530 ) ) ;
#8223 = ORIENTED_EDGE ( 'NONE', *, *, #2539, .F. ) ;
#8224 = CARTESIAN_POINT ( 'NONE',  ( 21.28817020210873423, 18.47861593500339694, 13.00425721518307576 ) ) ;
#8225 = AXIS2_PLACEMENT_3D ( 'NONE', #7312, #7262, #529 ) ;
#8226 = DIRECTION ( 'NONE',  ( -1.000000000000000000, -0.000000000000000000, -0.000000000000000000 ) ) ;
#8227 = DIRECTION ( 'NONE',  ( 0.000000000000000000, 2.312964634635742464E-16, 1.000000000000000000 ) ) ;
#8228 = CARTESIAN_POINT ( 'NONE',  ( 29.49999999999999645, -2.999999999999978240, -17.49999999999999645 ) ) ;
#8229 = AXIS2_PLACEMENT_3D ( 'NONE', #10856, #4864, #3966 ) ;
#8230 = CARTESIAN_POINT ( 'NONE',  ( 1.101703131577918438, 27.52740819067395606, 14.61156658473306713 ) ) ;
#8231 = CARTESIAN_POINT ( 'NONE',  ( 29.49999999999999645, 0.5000000000000135447, -4.999999999999991118 ) ) ;
#8232 = EDGE_CURVE ( 'NONE', #2863, #3414, #8125, .T. ) ;
#8233 = AXIS2_PLACEMENT_3D ( 'NONE', #1829, #5223, #10109 ) ;
#8234 = VERTEX_POINT ( 'NONE', #5172 ) ;
#8235 = LINE ( 'NONE', #9966, #3855 ) ;
#8236 = EDGE_CURVE ( 'NONE', #2061, #6902, #6123, .T. ) ;
#8237 = ORIENTED_EDGE ( 'NONE', *, *, #1729, .F. ) ;
#8238 = EDGE_CURVE ( 'NONE', #4566, #5004, #4397, .T. ) ;
#8239 = CARTESIAN_POINT ( 'NONE',  ( 1.515916693951008254, 33.47259180932604750, 14.57593341526694175 ) ) ;
#8240 = B_SPLINE_CURVE_WITH_KNOTS ( 'NONE', 3,
 ( #9428, #3655, #7204, #1265 ),
 .UNSPECIFIED., .F., .F.,
 ( 4, 4 ),
 ( 2.380739282171252709E-07, 0.002044882221487493313 ),
 .UNSPECIFIED. ) ;
#8241 = AXIS2_PLACEMENT_3D ( 'NONE', #6426, #423, #10551 ) ;
#8242 = DIRECTION ( 'NONE',  ( -0.000000000000000000, -0.000000000000000000, 1.000000000000000000 ) ) ;
#8243 = AXIS2_PLACEMENT_3D ( 'NONE', #3914, #7295, #9026 ) ;
#8244 = DIRECTION ( 'NONE',  ( 0.000000000000000000, 0.000000000000000000, 1.000000000000000000 ) ) ;
#8245 = AXIS2_PLACEMENT_3D ( 'NONE', #80, #1929, #969 ) ;
#8246 = CARTESIAN_POINT ( 'NONE',  ( 0.000000000000000000, 30.00000000000000000, -2.500000000000000000 ) ) ;
#8247 = DIRECTION ( 'NONE',  ( -1.000000000000000000, -0.000000000000000000, -0.000000000000000000 ) ) ;
#8248 = CARTESIAN_POINT ( 'NONE',  ( -24.35964822603314772, 55.55208333237727913, -5.935950539335252074 ) ) ;
#8249 = CARTESIAN_POINT ( 'NONE',  ( 2.805705207896068476, -3.226868319750173075, -3.503898532754370354 ) ) ;
#8250 = CARTESIAN_POINT ( 'NONE',  ( 3.999999999999998224, 2.472263674411418588, -3.687027874309861897 ) ) ;
#8251 = ADVANCED_FACE ( 'NONE', ( #1782 ), #8553, .F. ) ;
#8252 = VERTEX_POINT ( 'NONE', #879 ) ;
#8253 = CARTESIAN_POINT ( 'NONE',  ( 1.449747468305836673, 26.49999999999999289, 15.60937500000000533 ) ) ;
#8254 = AXIS2_PLACEMENT_3D ( 'NONE', #3370, #6628, #1644 ) ;
#8255 = DIRECTION ( 'NONE',  ( 0.000000000000000000, 0.000000000000000000, 1.000000000000000000 ) ) ;
#8256 = EDGE_CURVE ( 'NONE', #10104, #1107, #209, .T. ) ;
#8257 = CARTESIAN_POINT ( 'NONE',  ( -25.17020516978313083, 50.47708333237727629, -3.596074190997380349 ) ) ;
#8258 = CIRCLE ( 'NONE', #100, 4.999999999999997335 ) ;
#8259 = CARTESIAN_POINT ( 'NONE',  ( -25.98076211353310683, 52.34374999904395054, -3.128098921329806714 ) ) ;
#8260 = VECTOR ( 'NONE', #1574, 1000.000000000000000 ) ;
#8261 = CARTESIAN_POINT ( 'NONE',  ( 18.27511531525127353, 17.01097670698189290, 12.03680973694848966 ) ) ;
#8262 = CARTESIAN_POINT ( 'NONE',  ( -27.98076211353308551, 49.79166666666652930, -6.154700538379338504 ) ) ;
#8263 = ORIENTED_EDGE ( 'NONE', *, *, #1433, .T. ) ;
#8264 = CARTESIAN_POINT ( 'NONE',  ( -26.79131905728310059, 55.02708333237728056, -6.403925809002825709 ) ) ;
#8265 = ORIENTED_EDGE ( 'NONE', *, *, #1622, .T. ) ;
#8267 = ORIENTED_EDGE ( 'NONE', *, *, #6288, .F. ) ;
#8266 = EDGE_CURVE ( 'NONE', #1687, #7008, #6890, .T. ) ;
#8268 = DIRECTION ( 'NONE',  ( 0.000000000000000000, -1.000000000000000000, 0.000000000000000000 ) ) ;
#8269 = EDGE_LOOP ( 'NONE', ( #1079, #184 ) ) ;
#8270 = CARTESIAN_POINT ( 'NONE',  ( 1.767766952966372429, 31.76776695296637598, 16.00000000000000355 ) ) ;
#8271 = DIRECTION ( 'NONE',  ( 1.000000000000000000, 0.000000000000000000, 0.000000000000000000 ) ) ;
#8272 = ORIENTED_EDGE ( 'NONE', *, *, #8179, .F. ) ;
#8273 = CARTESIAN_POINT ( 'NONE',  ( 23.08245441082096150, 20.10811672198468969, 11.00732503135576401 ) ) ;
#8274 = CARTESIAN_POINT ( 'NONE',  ( 29.49999999999999645, 1.387778780781445676E-14, -12.49999999999999822 ) ) ;
#8275 = DIRECTION ( 'NONE',  ( -1.000000000000000000, -6.098637220230963674E-17, 0.000000000000000000 ) ) ;
#8276 = CARTESIAN_POINT ( 'NONE',  ( 19.34072721801214456, 22.67515267995686656, 12.94889058896629663 ) ) ;
#8277 = CARTESIAN_POINT ( 'NONE',  ( -23.98076211353314235, 50.11249999808803324, -5.000000000000103029 ) ) ;
#8278 = DIRECTION ( 'NONE',  ( -1.000000000000000000, 0.000000000000000000, -0.000000000000000000 ) ) ;
#8279 = CARTESIAN_POINT ( 'NONE',  ( -27.78268512908116961, 55.49961679590672503, -4.132201955500060642 ) ) ;
#8280 = ORIENTED_EDGE ( 'NONE', *, *, #10269, .T. ) ;
#8281 =( GEOMETRIC_REPRESENTATION_CONTEXT ( 3 ) GLOBAL_UNCERTAINTY_ASSIGNED_CONTEXT ( ( #2769 ) ) GLOBAL_UNIT_ASSIGNED_CONTEXT ( ( #10761, #3213, #8379 ) ) REPRESENTATION_CONTEXT ( 'NONE', 'WORKASPACE' ) );
#8282 = CARTESIAN_POINT ( 'NONE',  ( 2.474873734152918558, 32.47487373415292211, 13.50000000000000355 ) ) ;
#8283 = ORIENTED_EDGE ( 'NONE', *, *, #10711, .T. ) ;
#8284 = CARTESIAN_POINT ( 'NONE',  ( 23.02513694122459498, 21.97618599832468433, 13.00425721518307753 ) ) ;
#8285 = DIRECTION ( 'NONE',  ( 1.000000000000000000, 0.000000000000000000, 0.000000000000000000 ) ) ;
#8286 = CIRCLE ( 'NONE', #9895, 5.000000000000000888 ) ;
#8287 = DIRECTION ( 'NONE',  ( 0.000000000000000000, 0.000000000000000000, 1.000000000000000000 ) ) ;
#8288 = CARTESIAN_POINT ( 'NONE',  ( -1.317756351988340180, 3.857995168970202116, -0.04852650426601388955 ) ) ;
#8289 = ADVANCED_FACE ( 'NONE', ( #1046 ), #9437, .F. ) ;
#8290 = CARTESIAN_POINT ( 'NONE',  ( 1.720978244806805169, 31.81455566112594013, 13.75219158473306535 ) ) ;
#8291 = DIRECTION ( 'NONE',  ( -1.000000000000000000, -6.098637220230964906E-17, -6.308085367188384325E-16 ) ) ;
#8292 = ORIENTED_EDGE ( 'NONE', *, *, #3597, .T. ) ;
#8293 = DIRECTION ( 'NONE',  ( -0.8660254037844373753, 0.5000000000000021094, 0.000000000000000000 ) ) ;
#8294 = ORIENTED_EDGE ( 'NONE', *, *, #9732, .F. ) ;
#8295 = AXIS2_PLACEMENT_3D ( 'NONE', #9609, #10510, #3726 ) ;
#8296 = PRESENTATION_LAYER_ASSIGNMENT (  '', '', ( #6704 ) ) ;
#8297 = CARTESIAN_POINT ( 'NONE',  ( -26.98076211353309972, 52.06666666666653498, -3.267949192431252037 ) ) ;
#8298 = CARTESIAN_POINT ( 'NONE',  ( -4.000000000000000000, 2.471528634177585282, -3.686887442155186712 ) ) ;
#8299 = LINE ( 'NONE', #6463, #8598 ) ;
#8300 = LINE ( 'NONE', #9921, #3999 ) ;
#8301 = EDGE_CURVE ( 'NONE', #7385, #1406, #6996, .T. ) ;
#8302 = DIRECTION ( 'NONE',  ( 0.000000000000000000, 8.326672684688671588E-17, 1.000000000000000000 ) ) ;
#8303 = CARTESIAN_POINT ( 'NONE',  ( -27.60187600103308014, 55.08541666571061057, -5.935950539335252074 ) ) ;
#8304 = EDGE_CURVE ( 'NONE', #927, #7695, #3104, .T. ) ;
#8305 = DIRECTION ( 'NONE',  ( 0.000000000000000000, -1.000000000000000000, 9.783878858594328898E-16 ) ) ;
#8306 = COLOUR_RGB ( '', 0.72549020, 0.75294118, 0.79215686) ;
#8307 = CARTESIAN_POINT ( 'NONE',  ( 2.500000000000000000, 2.357898499370433054, -1.951563910473907981E-15 ) ) ;
#8308 = EDGE_LOOP ( 'NONE', ( #3131, #10612, #1855, #9766 ) ) ;
#8309 = CARTESIAN_POINT ( 'NONE',  ( 1.449747468305832898, 33.50000000000000000, 13.57812500000000533 ) ) ;
#8310 = CARTESIAN_POINT ( 'NONE',  ( -25.98076211353311393, 50.37499999999987210, -7.000000000000073719 ) ) ;
#8311 = CARTESIAN_POINT ( 'NONE',  ( -25.17020516978313083, 51.41041666571061342, -6.403925809002825709 ) ) ;
#8312 = ADVANCED_FACE ( 'NONE', ( #9491 ), #1892, .T. ) ;
#8313 = CARTESIAN_POINT ( 'NONE',  ( -26.79131905728310059, 53.45208333237728482, -6.403925809002825709 ) ) ;
#8314 = CARTESIAN_POINT ( 'NONE',  ( 22.98009469009668138, 21.94211999725310491, 12.00579112326941988 ) ) ;
#8315 =( BOUNDED_CURVE ( )  B_SPLINE_CURVE ( 2, ( #3421, #5204, #6079, #1640, #5035, #4311, #9468, #792, #7699 ),
 .UNSPECIFIED., .F., .F. ) 
 B_SPLINE_CURVE_WITH_KNOTS ( ( 3, 2, 2, 2, 3 ),
 ( 0.8611111111111111605, 0.8703703703703703498, 0.8888888888888888395, 0.9074074074074074403, 0.9166666666666666297 ),
 .UNSPECIFIED. ) 
 CURVE ( )  GEOMETRIC_REPRESENTATION_ITEM ( )  RATIONAL_B_SPLINE_CURVE ( ( 0.9330127018922194093, 0.9330127018922197424, 1.000000000000000000, 0.8660254037844387076, 1.000000000000000000, 0.8660254037844387076, 1.000000000000000000, 0.9330127018922197424, 0.9330127018922194093 ) ) 
 REPRESENTATION_ITEM ( '' )  );
#8316 = CARTESIAN_POINT ( 'NONE',  ( -24.98076211353313170, 51.48333333333319928, -3.267949192431250705 ) ) ;
#8317 = ORIENTED_EDGE ( 'NONE', *, *, #1459, .F. ) ;
#8318 = EDGE_CURVE ( 'NONE', #5165, #5356, #5942, .T. ) ;
#8319 = EDGE_CURVE ( 'NONE', #2261, #4849, #86, .T. ) ;
#8320 = FILL_AREA_STYLE_COLOUR ( '', #4771 ) ;
#8321 = ORIENTED_EDGE ( 'NONE', *, *, #2623, .T. ) ;
#8322 = VERTEX_POINT ( 'NONE', #8440 ) ;
#8323 = CARTESIAN_POINT ( 'NONE',  ( 0.000000000000000000, -3.031088913245509886, 1.750000000000043077 ) ) ;
#8324 = ORIENTED_EDGE ( 'NONE', *, *, #2477, .F. ) ;
#8325 = CARTESIAN_POINT ( 'NONE',  ( -2.469212770973128190, 29.60886282244813117, 16.49922112211940117 ) ) ;
#8326 = DIRECTION ( 'NONE',  ( 6.982962677686266711E-15, 0.000000000000000000, -1.000000000000000000 ) ) ;
#8327 = VERTEX_POINT ( 'NONE', #6770 ) ;
#8328 = CARTESIAN_POINT ( 'NONE',  ( 20.28019557727208166, 19.74811736329550982, 11.00732503135576401 ) ) ;
#8329 = DIRECTION ( 'NONE',  ( 0.000000000000000000, 0.000000000000000000, 1.000000000000000000 ) ) ;
#8330 = CARTESIAN_POINT ( 'NONE',  ( 2.982579934988244030, -3.876582599186213063, 0.2855619784720940246 ) ) ;
#8331 = CARTESIAN_POINT ( 'NONE',  ( 21.33748252609158058, 23.71725136694109892, 12.94889058896590583 ) ) ;
#8332 = CARTESIAN_POINT ( 'NONE',  ( -23.98076211353314235, 53.61249999808804034, -5.000000000000103029 ) ) ;
#8333 = CARTESIAN_POINT ( 'NONE',  ( 4.000000000000000000, -2.309401076758516691, -0.4999999999999995559 ) ) ;
#8334 = FACE_OUTER_BOUND ( 'NONE', #1295, .T. ) ;
#8335 = PRODUCT_DEFINITION_CONTEXT ( 'detailed design', #10047, 'design' ) ;
#8336 = EDGE_LOOP ( 'NONE', ( #9889, #9625, #1961, #8812 ) ) ;
#8337 = CARTESIAN_POINT ( 'NONE',  ( -3.500000000000002220, 28.55025253169416288, 14.04687500000000355 ) ) ;
#8338 = VERTEX_POINT ( 'NONE', #10168 ) ;
#8339 = EDGE_CURVE ( 'NONE', #7488, #8693, #2554, .T. ) ;
#8340 = CARTESIAN_POINT ( 'NONE',  ( 23.38258886820915095, 18.73219245557438484, 12.94889058896590583 ) ) ;
#8341 = EDGE_CURVE ( 'NONE', #5356, #5165, #4360, .T. ) ;
#8342 = CARTESIAN_POINT ( 'NONE',  ( 20.65761543282678758, 16.89116807672653664, 11.95042449705224819 ) ) ;
#8343 = CYLINDRICAL_SURFACE ( 'NONE', #10096, 2.649999999999991029 ) ;
#8344 = CARTESIAN_POINT ( 'NONE',  ( -0.6507732100473471171, 4.243078065514775510, -0.2236248678334823436 ) ) ;
#8345 = CARTESIAN_POINT ( 'NONE',  ( 1.383578242660657098, 33.52740819067396671, 13.83031658473306535 ) ) ;
#8346 = CARTESIAN_POINT ( 'NONE',  ( -23.98076211353314235, 51.45416666475470180, -3.845299461620867554 ) ) ;
#8347 = DIRECTION ( 'NONE',  ( -6.098637220230963674E-17, 1.000000000000000000, 0.000000000000000000 ) ) ;
#8348 = CARTESIAN_POINT ( 'NONE',  ( 3.169801662054985592, 0.6882444255504213126, 3.499999999999999556 ) ) ;
#8349 = EDGE_LOOP ( 'NONE', ( #4425, #431, #7222, #4627 ) ) ;
#8350 = ORIENTED_EDGE ( 'NONE', *, *, #1546, .T. ) ;
#8351 = CARTESIAN_POINT ( 'NONE',  ( 0.6507732100473444525, -4.243078065514795050, -0.2236248678334952777 ) ) ;
#8352 = VECTOR ( 'NONE', #10361, 1000.000000000000000 ) ;
#8353 = CARTESIAN_POINT ( 'NONE',  ( -4.000000000000000000, -0.8232339106130515116, -3.430630286862743183 ) ) ;
#8354 = CARTESIAN_POINT ( 'NONE',  ( 20.00651627240589647, 19.97666299463432438, 12.00579112326824216 ) ) ;
#8355 = CARTESIAN_POINT ( 'NONE',  ( 4.203833317240879275, 1.627343821129582979, -3.597273115243889929 ) ) ;
#8356 = DIRECTION ( 'NONE',  ( 0.000000000000000000, 0.000000000000000000, -1.000000000000000000 ) ) ;
#8357 = CARTESIAN_POINT ( 'NONE',  ( -27.60187600103308370, 50.06874999904395196, -5.000000000000103029 ) ) ;
#8358 = CARTESIAN_POINT ( 'NONE',  ( -5.560781378645575757, 6.809993116116508640E-16, -4.000000000000000000 ) ) ;
#8359 = LINE ( 'NONE', #5039, #6309 ) ;
#8360 = AXIS2_PLACEMENT_3D ( 'NONE', #1629, #5026, #8398 ) ;
#8361 = ORIENTED_EDGE ( 'NONE', *, *, #8499, .T. ) ;
#8362 = CARTESIAN_POINT ( 'NONE',  ( 1.035533905932743970, 27.49999999999999289, 14.35937500000000711 ) ) ;
#8363 = FACE_OUTER_BOUND ( 'NONE', #2916, .T. ) ;
#8364 = EDGE_CURVE ( 'NONE', #1566, #2863, #7356, .T. ) ;
#8365 = CARTESIAN_POINT ( 'NONE',  ( -27.60187600103308370, 50.24374999904394912, -5.000000000000103029 ) ) ;
#8366 = CARTESIAN_POINT ( 'NONE',  ( -25.17020516978313083, 54.50208333237728198, -3.596074190997380349 ) ) ;
#8367 = CARTESIAN_POINT ( 'NONE',  ( 17.65010306112908722, 17.31038946799904465, 12.07741653513508417 ) ) ;
#8368 = CARTESIAN_POINT ( 'NONE',  ( -26.98076211353309972, 53.46666666666653356, -3.267949192431252037 ) ) ;
#8369 = CIRCLE ( 'NONE', #2714, 2.149999999999992362 ) ;
#8370 = VERTEX_POINT ( 'NONE', #6263 ) ;
#8371 = ADVANCED_FACE ( 'NONE', ( #9771, #9657 ), #422, .T. ) ;
#8372 = EDGE_CURVE ( 'NONE', #10564, #7610, #1149, .T. ) ;
#8373 = ORIENTED_EDGE ( 'NONE', *, *, #9322, .T. ) ;
#8374 = ORIENTED_EDGE ( 'NONE', *, *, #1624, .F. ) ;
#8375 = CARTESIAN_POINT ( 'NONE',  ( 21.21106610644839208, 53.49999999999983658, 2.500000000000000000 ) ) ;
#8377 = ORIENTED_EDGE ( 'NONE', *, *, #10764, .F. ) ;
#8376 = ADVANCED_FACE ( 'NONE', ( #10660 ), #4504, .F. ) ;
#8378 = DIRECTION ( 'NONE',  ( 1.000000000000000000, 0.000000000000000000, 0.000000000000000000 ) ) ;
#8379 =( NAMED_UNIT ( * ) SI_UNIT ( $, .STERADIAN. ) SOLID_ANGLE_UNIT ( ) );
#8380 = ORIENTED_EDGE ( 'NONE', *, *, #4038, .F. ) ;
#8381 = CARTESIAN_POINT ( 'NONE',  ( 22.99824548812224378, 19.95783898428147651, 11.00732503135576401 ) ) ;
#8382 = DIRECTION ( 'NONE',  ( -0.000000000000000000, -0.000000000000000000, -1.000000000000000000 ) ) ;
#8383 =( BOUNDED_CURVE ( )  B_SPLINE_CURVE ( 2, ( #7787, #1047, #2619, #163, #3559, #2728, #6101, #9493, #4456 ),
 .UNSPECIFIED., .F., .F. ) 
 B_SPLINE_CURVE_WITH_KNOTS ( ( 3, 2, 2, 2, 3 ),
 ( 0.7500000000000000000, 0.7592592592592593004, 0.7777777777777777901, 0.7962962962962962798, 0.8055555555555555802 ),
 .UNSPECIFIED. ) 
 CURVE ( )  GEOMETRIC_REPRESENTATION_ITEM ( )  RATIONAL_B_SPLINE_CURVE ( ( 0.9330127018922194093, 0.9330127018922194093, 1.000000000000000000, 0.8660254037844387076, 1.000000000000000000, 0.8660254037844387076, 1.000000000000000000, 0.9330127018922189652, 0.9330127018922194093 ) ) 
 REPRESENTATION_ITEM ( '' )  );
#8384 = CARTESIAN_POINT ( 'NONE',  ( 2.000000000000000000, 0.000000000000000000, 0.000000000000000000 ) ) ;
#8385 = CARTESIAN_POINT ( 'NONE',  ( 16.72700999897183038, 16.80849948458634557, 12.09707671258119888 ) ) ;
#8386 = B_SPLINE_CURVE_WITH_KNOTS ( 'NONE', 1,
 ( #5123, #881 ),
 .UNSPECIFIED., .F., .F.,
 ( 2, 2 ),
 ( 0.000000000000000000, 1.000000000000000000 ),
 .UNSPECIFIED. ) ;
#8387 = CARTESIAN_POINT ( 'NONE',  ( 0.1999999999999987899, 0.000000000000000000, 0.000000000000000000 ) ) ;
#8388 = CARTESIAN_POINT ( 'NONE',  ( -25.98076211353311393, 55.53749999808803750, -2.690598923241634743 ) ) ;
#8389 = DIRECTION ( 'NONE',  ( 0.000000000000000000, 0.000000000000000000, -1.000000000000000000 ) ) ;
#8390 = ORIENTED_EDGE ( 'NONE', *, *, #4046, .T. ) ;
#8391 = CARTESIAN_POINT ( 'NONE',  ( 29.50000000000000711, 2.000000000000001776, -12.50000000000000000 ) ) ;
#8392 = ORIENTED_EDGE ( 'NONE', *, *, #685, .F. ) ;
#8393 = CARTESIAN_POINT ( 'NONE',  ( -1.449747468305830678, 26.49999999999999289, 14.20312500000000355 ) ) ;
#8394 = EDGE_LOOP ( 'NONE', ( #4734, #6267, #5522, #5306 ) ) ;
#8395 = CARTESIAN_POINT ( 'NONE',  ( 23.22159451225019566, 21.65168511467167889, 13.00425721518366728 ) ) ;
#8396 = CARTESIAN_POINT ( 'NONE',  ( -25.98076211353311393, 49.49999999999986500, -3.000000000000131894 ) ) ;
#8397 = CARTESIAN_POINT ( 'NONE',  ( 2.000000000000000000, 1.773042676681340524, -2.059984127722458425E-15 ) ) ;
#8398 = DIRECTION ( 'NONE',  ( 1.000000000000000000, 0.000000000000000000, 0.000000000000000000 ) ) ;
#8399 = CARTESIAN_POINT ( 'NONE',  ( -0.06616922564517727090, 32.50000000000000711, 15.15844158473306535 ) ) ;
#8400 = CARTESIAN_POINT ( 'NONE',  ( 0.2500000000000002220, 5.204748896376250699E-16, -4.250000000000000000 ) ) ;
#8401 = LINE ( 'NONE', #3356, #1682 ) ;
#8402 = DIRECTION ( 'NONE',  ( -1.000000000000000000, 0.000000000000000000, 0.000000000000000000 ) ) ;
#8403 = ORIENTED_EDGE ( 'NONE', *, *, #6049, .T. ) ;
#8404 = ORIENTED_EDGE ( 'NONE', *, *, #9617, .F. ) ;
#8405 = AXIS2_PLACEMENT_3D ( 'NONE', #10713, #4733, #8110 ) ;
#8406 = EDGE_CURVE ( 'NONE', #1703, #3863, #5444, .T. ) ;
#8407 = DIRECTION ( 'NONE',  ( 0.000000000000000000, 1.000000000000000000, 0.000000000000000000 ) ) ;
#8408 = DIRECTION ( 'NONE',  ( 0.000000000000000000, 1.000000000000000000, 0.000000000000000000 ) ) ;
#8409 = CARTESIAN_POINT ( 'NONE',  ( 34.64101615137754209, 5.000000000000001776, -2.500000000000000000 ) ) ;
#8410 = CARTESIAN_POINT ( 'NONE',  ( -2.500000000000004441, 28.96446609406725514, 15.29687500000000533 ) ) ;
#8411 = CARTESIAN_POINT ( 'NONE',  ( 34.85586774767502760, 3.177316488306996423, 3.109148447068123655 ) ) ;
#8412 = CARTESIAN_POINT ( 'NONE',  ( -26.79131905728310059, 50.18541666571061199, -3.596074190997381237 ) ) ;
#8413 = AXIS2_PLACEMENT_3D ( 'NONE', #5935, #6884, #2670 ) ;
#8414 = DIRECTION ( 'NONE',  ( -1.000000000000000000, -0.000000000000000000, -0.000000000000000000 ) ) ;
#8415 = CARTESIAN_POINT ( 'NONE',  ( 4.211399257449709665, -2.459727064652517114, -3.751161691472417736 ) ) ;
#8416 = ORIENTED_EDGE ( 'NONE', *, *, #1654, .F. ) ;
#8417 = CARTESIAN_POINT ( 'NONE',  ( -25.98076211353311393, 50.72499999999985931, -3.000000000000132783 ) ) ;
#8418 = VECTOR ( 'NONE', #10849, 1000.000000000000000 ) ;
#8419 = CARTESIAN_POINT ( 'NONE',  ( -27.98076211353308551, 53.20416666475470180, -6.154700538379338504 ) ) ;
#8420 = VECTOR ( 'NONE', #9878, 1000.000000000000000 ) ;
#8421 = CARTESIAN_POINT ( 'NONE',  ( -26.79131905728310059, 52.46041666571061768, -3.596074190997381237 ) ) ;
#8422 = LINE ( 'NONE', #1821, #1691 ) ;
#8423 = VECTOR ( 'NONE', #1156, 1000.000000000000000 ) ;
#8424 = CIRCLE ( 'NONE', #10025, 30.00000000000000000 ) ;
#8425 = DIRECTION ( 'NONE',  ( 0.000000000000000000, 0.000000000000000000, 1.000000000000000000 ) ) ;
#8426 = CARTESIAN_POINT ( 'NONE',  ( -27.98076211353308551, 51.19166666666652787, -6.154700538379338504 ) ) ;
#8427 = TOROIDAL_SURFACE ( 'NONE', #4719, 3.369999999999997886, 0.1199999999999999956 ) ;
#8428 = AXIS2_PLACEMENT_3D ( 'NONE', #9831, #6388, #6433 ) ;
#8429 = ORIENTED_EDGE ( 'NONE', *, *, #2031, .T. ) ;
#8430 = EDGE_CURVE ( 'NONE', #990, #7845, #2413, .T. ) ;
#8431 = ORIENTED_EDGE ( 'NONE', *, *, #6409, .T. ) ;
#8432 = EDGE_LOOP ( 'NONE', ( #2961, #4078, #7888, #2631 ) ) ;
#8433 = CARTESIAN_POINT ( 'NONE',  ( 27.50000000000001066, -8.499999999999985789, -4.999999999999992006 ) ) ;
#8434 = ORIENTED_EDGE ( 'NONE', *, *, #8808, .T. ) ;
#8435 = DIRECTION ( 'NONE',  ( -1.000000000000000000, 0.000000000000000000, 0.000000000000000000 ) ) ;
#8436 = DIRECTION ( 'NONE',  ( -1.000000000000000000, 0.000000000000000000, -6.982962677686266711E-15 ) ) ;
#8437 = EDGE_LOOP ( 'NONE', ( #5878, #2340, #6605 ) ) ;
#8438 =( BOUNDED_CURVE ( )  B_SPLINE_CURVE ( 2, ( #6685, #4307, #7697, #3475, #7464, #10084, #8297, #682, #2473 ),
 .UNSPECIFIED., .F., .F. ) 
 B_SPLINE_CURVE_WITH_KNOTS ( ( 3, 2, 2, 2, 3 ),
 ( 0.3611111111111111049, 0.3703703703703703498, 0.3888888888888888951, 0.4074074074074073848, 0.4166666666666666297 ),
 .UNSPECIFIED. ) 
 CURVE ( )  GEOMETRIC_REPRESENTATION_ITEM ( )  RATIONAL_B_SPLINE_CURVE ( ( 0.9330127018922194093, 0.9330127018922194093, 1.000000000000000000, 0.8660254037844387076, 1.000000000000000000, 0.8660254037844387076, 1.000000000000000000, 0.9330127018922196314, 0.9330127018922194093 ) ) 
 REPRESENTATION_ITEM ( '' )  );
#8439 = CARTESIAN_POINT ( 'NONE',  ( 18.06244887585786074, 17.10054717930957224, 11.04774946733758512 ) ) ;
#8440 = CARTESIAN_POINT ( 'NONE',  ( 2.500000000000000444, 0.000000000000000000, -5.000000000000000888 ) ) ;
#8441 = AXIS2_PLACEMENT_3D ( 'NONE', #8916, #7346, #3860 ) ;
#8442 =( LENGTH_UNIT ( ) NAMED_UNIT ( * ) SI_UNIT ( .MILLI., .METRE. ) );
#8443 = CARTESIAN_POINT ( 'NONE',  ( -26.79131905728310059, 50.36041666571060915, -3.596074190997381237 ) ) ;
#8444 = EDGE_CURVE ( 'NONE', #6740, #10232, #10550, .T. ) ;
#8445 = CARTESIAN_POINT ( 'NONE',  ( 22.96512898726170704, 23.28924158689358848, 11.95042449705224819 ) ) ;
#8446 = DIRECTION ( 'NONE',  ( -0.000000000000000000, 0.000000000000000000, -1.000000000000000000 ) ) ;
#8447 = EDGE_CURVE ( 'NONE', #9319, #6022, #9552, .T. ) ;
#8448 = CARTESIAN_POINT ( 'NONE',  ( -25.17020516978313083, 50.01041666571061484, -6.403925809002825709 ) ) ;
#8449 = AXIS2_PLACEMENT_3D ( 'NONE', #8, #10185, #2580 ) ;
#8450 = CARTESIAN_POINT ( 'NONE',  ( -21.21106610644865498, 16.50000000000026290, -5.000000000000000000 ) ) ;
#8451 = ORIENTED_EDGE ( 'NONE', *, *, #8364, .F. ) ;
#8452 = CARTESIAN_POINT ( 'NONE',  ( -25.47444609516507441, 58.87210758029105762, -3.061288170098404926 ) ) ;
#8453 = ORIENTED_EDGE ( 'NONE', *, *, #5493, .T. ) ;
#8454 = CARTESIAN_POINT ( 'NONE',  ( 3.903127820947815962E-15, 26.49999999999999289, 15.53125000000000355 ) ) ;
#8455 = ORIENTED_EDGE ( 'NONE', *, *, #9566, .F. ) ;
#8456 = CARTESIAN_POINT ( 'NONE',  ( 22.47009348518006888, 19.30075366110858326, 13.00425721518280042 ) ) ;
#8457 = EDGE_CURVE ( 'NONE', #7380, #647, #3826, .T. ) ;
#8458 = CARTESIAN_POINT ( 'NONE',  ( 16.90694777372845437, 16.62861179130368683, 12.08020438729360180 ) ) ;
#8459 = LINE ( 'NONE', #7630, #2156 ) ;
#8460 = CARTESIAN_POINT ( 'NONE',  ( -27.60187600103308014, 52.22708333237728340, -4.064049460664955760 ) ) ;
#8461 = CARTESIAN_POINT ( 'NONE',  ( -2.500000000000004441, 28.96446609406725159, 15.29687500000000178 ) ) ;
#8462 = PRODUCT_DEFINITION_FORMATION_WITH_SPECIFIED_SOURCE ( 'ANY', '', #9880, .NOT_KNOWN. ) ;
#8463 = CARTESIAN_POINT ( 'NONE',  ( 0.2500000000000002220, 0.000000000000000000, 0.000000000000000000 ) ) ;
#8464 = DIRECTION ( 'NONE',  ( -0.5150380749100518241, 1.049727191138620421E-16, -0.8571673007021137769 ) ) ;
#8465 = CARTESIAN_POINT ( 'NONE',  ( 4.200000000000001954, 0.000000000000000000, -2.200000000000001066 ) ) ;
#8466 = EDGE_CURVE ( 'NONE', #9720, #3725, #6323, .T. ) ;
#8467 = EDGE_LOOP ( 'NONE', ( #6488, #3322 ) ) ;
#8468 = ORIENTED_EDGE ( 'NONE', *, *, #7654, .F. ) ;
#8469 = CARTESIAN_POINT ( 'NONE',  ( -25.98076211353311393, 49.49999999999986500, -5.000000000000103029 ) ) ;
#8470 = CARTESIAN_POINT ( 'NONE',  ( 0.000000000000000000, 0.000000000000000000, -4.000000000000000000 ) ) ;
#8471 = CIRCLE ( 'NONE', #2445, 2.649999999999991029 ) ;
#8472 = CARTESIAN_POINT ( 'NONE',  ( 22.44007493706583745, 19.34731747087121434, 12.00579112326928133 ) ) ;
#8473 = CARTESIAN_POINT ( 'NONE',  ( -1.035533905932742860, 32.50000000000000000, 14.98437500000000533 ) ) ;
#8474 = CARTESIAN_POINT ( 'NONE',  ( 34.80692069235085029, 3.675807134350210337, 2.800930295893637734 ) ) ;
#8475 = CARTESIAN_POINT ( 'NONE',  ( -25.98076211353311393, 52.69374999904394485, -6.871901078670400231 ) ) ;
#8476 = EDGE_CURVE ( 'NONE', #3879, #7957, #3822, .T. ) ;
#8477 = FACE_OUTER_BOUND ( 'NONE', #82, .T. ) ;
#8478 = CARTESIAN_POINT ( 'NONE',  ( 29.49999999999999289, 2.000000000000001776, 17.50000000000000000 ) ) ;
#8479 = DIRECTION ( 'NONE',  ( -1.000000000000000000, 0.000000000000000000, 0.000000000000000000 ) ) ;
#8480 = ORIENTED_EDGE ( 'NONE', *, *, #1769, .F. ) ;
#8481 = CARTESIAN_POINT ( 'NONE',  ( -4.211140560182196957, -2.431303136016552013, -3.745885042887436178 ) ) ;
#8482 = CARTESIAN_POINT ( 'NONE',  ( 24.99999259214812142, 30.01924558493218598, 2.500000000000000000 ) ) ;
#8483 = CARTESIAN_POINT ( 'NONE',  ( -26.79131905728310059, 54.56041666571061199, -3.596074190997381237 ) ) ;
#8484 = CARTESIAN_POINT ( 'NONE',  ( -27.60187600103308014, 55.69181177618368395, -4.629976867109323990 ) ) ;
#8485 = CIRCLE ( 'NONE', #8130, 34.99999999999999289 ) ;
#8486 = PRESENTATION_LAYER_ASSIGNMENT (  '', '', ( #5654 ) ) ;
#8487 = DIRECTION ( 'NONE',  ( -1.000000000000000000, 2.212882687011047826E-16, 0.000000000000000000 ) ) ;
#8488 = CARTESIAN_POINT ( 'NONE',  ( -24.98076211353312814, 52.41666666666652930, -6.732050807568954909 ) ) ;
#8489 = VERTEX_POINT ( 'NONE', #1218 ) ;
#8490 = ORIENTED_EDGE ( 'NONE', *, *, #9812, .T. ) ;
#8491 = CARTESIAN_POINT ( 'NONE',  ( 34.99999999999999289, -3.999999999999993339, 10.00000000000000533 ) ) ;
#8492 = ORIENTED_EDGE ( 'NONE', *, *, #3844, .F. ) ;
#8493 = DIRECTION ( 'NONE',  ( 0.000000000000000000, 0.000000000000000000, -1.000000000000000000 ) ) ;
#8494 = CARTESIAN_POINT ( 'NONE',  ( 0.000000000000000000, 0.000000000000000000, 0.000000000000000000 ) ) ;
#8495 = ORIENTED_EDGE ( 'NONE', *, *, #7977, .T. ) ;
#8496 = ADVANCED_FACE ( 'NONE', ( #7212 ), #8002, .F. ) ;
#8497 = CARTESIAN_POINT ( 'NONE',  ( 0.000000000000000000, 0.000000000000000000, -4.974599999999998801 ) ) ;
#8498 = CARTESIAN_POINT ( 'NONE',  ( 0.000000000000000000, 0.000000000000000000, 2.500000000000000000 ) ) ;
#8499 = EDGE_CURVE ( 'NONE', #10824, #3903, #10606, .T. ) ;
#8500 = CARTESIAN_POINT ( 'NONE',  ( -27.98076211353308551, 51.86249999808803324, -5.000000000000103029 ) ) ;
#8501 = CARTESIAN_POINT ( 'NONE',  ( 27.50000000000001066, 0.5000000000000134337, -4.999999999999992006 ) ) ;
#8502 = CARTESIAN_POINT ( 'NONE',  ( 21.27550008773165047, 17.38841780631423362, 10.95195840513859231 ) ) ;
#8503 = CARTESIAN_POINT ( 'NONE',  ( -2.682243648011671588, -3.070208061305317759, -0.04852650426602272971 ) ) ;
#8504 = LINE ( 'NONE', #6775, #3535 ) ;
#8505 = CARTESIAN_POINT ( 'NONE',  ( -27.98076211353308551, 55.30416666475468901, -6.154700538379338504 ) ) ;
#8506 = DIRECTION ( 'NONE',  ( 1.000000000000000000, -9.251858538542971828E-16, 0.000000000000000000 ) ) ;
#8507 = ORIENTED_EDGE ( 'NONE', *, *, #20, .F. ) ;
#8508 = CARTESIAN_POINT ( 'NONE',  ( -25.98076211353311393, 50.63749999808803892, -3.000000000000132339 ) ) ;
#8509 =( BOUNDED_SURFACE ( )  B_SPLINE_SURFACE ( 3, 2, ( 
 ( #2999, #10700, #6376 ),
 ( #1316, #5546, #3094 ),
 ( #8927, #4714, #8095 ),
 ( #7259, #5597, #6471 ),
 ( #2260, #10654, #3044 ),
 ( #5655, #1427, #6418 ) ),
 .UNSPECIFIED., .F., .F., .F. ) 
 B_SPLINE_SURFACE_WITH_KNOTS ( ( 4, 2, 4 ),
 ( 3, 3 ),
 ( 0.02032853247518126918, 0.02278863295364821906, 0.02524873343211516893 ),
 ( 0.000000000000000000, 1.000000000000000000 ),
 .UNSPECIFIED. ) 
 GEOMETRIC_REPRESENTATION_ITEM ( )  RATIONAL_B_SPLINE_SURFACE ( (
 ( 1.000000000000000000, 0.8047781615896838492, 1.000000000000000000),
 ( 1.000000000000000000, 0.8123767586288186404, 1.000000000000000000),
 ( 1.000000000000000000, 0.8190662415565814758, 1.000000000000000000),
 ( 1.000000000000000000, 0.8192361015667604107, 1.000000000000000000),
 ( 1.000000000000000000, 0.8126135807104967190, 1.000000000000000000),
 ( 1.000000000000000000, 0.8047712338318580017, 1.000000000000000000) ) ) 
 REPRESENTATION_ITEM ( '' )  SURFACE ( )  );
#8510 = ORIENTED_EDGE ( 'NONE', *, *, #4990, .F. ) ;
#8511 = CARTESIAN_POINT ( 'NONE',  ( -1.383578242660655100, 26.47259180932604039, 14.45531658473306535 ) ) ;
#8512 = PRODUCT_RELATED_PRODUCT_CATEGORY ( 'part', '', ( #5016 ) ) ;
#8513 = ORIENTED_EDGE ( 'NONE', *, *, #2889, .F. ) ;
#8514 = EDGE_CURVE ( 'NONE', #9774, #4274, #9176, .T. ) ;
#8515 = CARTESIAN_POINT ( 'NONE',  ( 20.55933174294505861, 16.75535677129292722, 12.94889058896590583 ) ) ;
#8516 =( NAMED_UNIT ( * ) SI_UNIT ( $, .STERADIAN. ) SOLID_ANGLE_UNIT ( ) );
#8517 = ADVANCED_FACE ( 'NONE', ( #1952 ), #6382, .T. ) ;
#8518 = DIRECTION ( 'NONE',  ( -0.000000000000000000, 0.000000000000000000, 1.000000000000000000 ) ) ;
#8519 = CARTESIAN_POINT ( 'NONE',  ( 18.62184541094303114, 16.98042197548449295, 12.02177981800743112 ) ) ;
#8520 = CARTESIAN_POINT ( 'NONE',  ( -25.98076211353415843, 59.00000000000900968, -2.999999999996041389 ) ) ;
#8521 = CARTESIAN_POINT ( 'NONE',  ( 1.767766952966377314, 28.23223304703363112, 14.43750000000000178 ) ) ;
#8522 = CARTESIAN_POINT ( 'NONE',  ( 16.58601566935799454, 18.36373179894816943, 12.17661548709639696 ) ) ;
#8523 = CARTESIAN_POINT ( 'NONE',  ( 2.499999999999999556, 0.000000000000000000, 3.469446951953614189E-15 ) ) ;
#8524 = CARTESIAN_POINT ( 'NONE',  ( 2.500000000000000000, 2.357898499370433054, -1.951563910473907981E-15 ) ) ;
#8525 = VERTEX_POINT ( 'NONE', #1154 ) ;
#8526 = EDGE_CURVE ( 'NONE', #6952, #1362, #8958, .T. ) ;
#8527 = ORIENTED_EDGE ( 'NONE', *, *, #7096, .F. ) ;
#8528 = ADVANCED_FACE ( 'NONE', ( #4037 ), #8156, .F. ) ;
#8529 = LINE ( 'NONE', #7580, #1167 ) ;
#8530 = CARTESIAN_POINT ( 'NONE',  ( -4.000000000000000000, 2.309401076758498483, -3.433295621305379353 ) ) ;
#8531 = CARTESIAN_POINT ( 'NONE',  ( 34.94281041931228771, 2.000000000000002220, -5.500000000000000000 ) ) ;
#8532 = CARTESIAN_POINT ( 'NONE',  ( 4.553649124439118623E-15, 27.49999999999999289, 15.53125000000000355 ) ) ;
#8533 = DIRECTION ( 'NONE',  ( 0.000000000000000000, -1.000000000000000000, 0.000000000000000000 ) ) ;
#8534 = CARTESIAN_POINT ( 'NONE',  ( -25.98076211353311393, 53.04374999904395338, -3.128098921329806714 ) ) ;
#8535 = LINE ( 'NONE', #1699, #3001 ) ;
#8536 = CARTESIAN_POINT ( 'NONE',  ( 26.25045812061784289, 56.49999999999984368, 14.50000000000000000 ) ) ;
#8537 = CARTESIAN_POINT ( 'NONE',  ( 2.887392608830372964, -2.020725942163647648, 3.499999999999999556 ) ) ;
#8538 = ORIENTED_EDGE ( 'NONE', *, *, #5387, .F. ) ;
#8539 = CARTESIAN_POINT ( 'NONE',  ( -4.197393957002303999, -0.8151795401431414234, -3.503767560748935139 ) ) ;
#8540 = DIRECTION ( 'NONE',  ( 0.000000000000000000, -0.000000000000000000, -1.000000000000000000 ) ) ;
#8541 = CIRCLE ( 'NONE', #5657, 1.999999999999971356 ) ;
#8542 = CARTESIAN_POINT ( 'NONE',  ( -25.17020516978313083, 54.91041666571061342, -6.403925809002825709 ) ) ;
#8543 = DIRECTION ( 'NONE',  ( -1.000000000000000000, -0.000000000000000000, -0.000000000000000000 ) ) ;
#8544 = CIRCLE ( 'NONE', #6048, 4.250000000000000000 ) ;
#8545 = CARTESIAN_POINT ( 'NONE',  ( 16.23246227876473213, 18.01017840835489991, 12.17661548709639696 ) ) ;
#8546 = CARTESIAN_POINT ( 'NONE',  ( -23.98076211353314235, 50.95833333333318649, -6.154700538379337615 ) ) ;
#8547 = ORIENTED_EDGE ( 'NONE', *, *, #460, .F. ) ;
#8548 = ORIENTED_EDGE ( 'NONE', *, *, #10280, .T. ) ;
#8549 = CARTESIAN_POINT ( 'NONE',  ( 3.170625919164804518, -0.6808742863896959374, -3.500000000000000000 ) ) ;
#8550 = APPLICATION_PROTOCOL_DEFINITION ( 'draft international standard', 'automotive_design', 1998, #5515 ) ;
#8551 = ORIENTED_EDGE ( 'NONE', *, *, #8672, .F. ) ;
#8552 = CARTESIAN_POINT ( 'NONE',  ( 20.05579831881754060, 20.86490736922957367, 14.50000000000000000 ) ) ;
#8553 = CYLINDRICAL_SURFACE ( 'NONE', #6297, 24.99999999999999645 ) ;
#8554 = DIRECTION ( 'NONE',  ( -0.000000000000000000, 1.000000000000000000, -0.000000000000000000 ) ) ;
#8555 = CARTESIAN_POINT ( 'NONE',  ( 1.047444401652940007E-13, 30.00000000000000000, 2.500000000000000000 ) ) ;
#8556 = CARTESIAN_POINT ( 'NONE',  ( 21.30711663910541276, 17.34296610691914253, 11.95042449705224819 ) ) ;
#8557 = PLANE ( 'NONE',  #7317 ) ;
#8558 = CARTESIAN_POINT ( 'NONE',  ( -27.60187600103308014, 50.18541666571061199, -5.935950539335252074 ) ) ;
#8559 = CARTESIAN_POINT ( 'NONE',  ( -24.98076211353312814, 53.81666666666652787, -6.732050807568954909 ) ) ;
#8560 = EDGE_LOOP ( 'NONE', ( #10289, #7452, #8794, #7194, #4154 ) ) ;
#8561 = CARTESIAN_POINT ( 'NONE',  ( 2.500000000000000000, 0.000000000000000000, 0.000000000000000000 ) ) ;
#8562 = VERTEX_POINT ( 'NONE', #7425 ) ;
#8563 = CARTESIAN_POINT ( 'NONE',  ( 2.521662442312487151, 27.57191497400665270, 13.43969158473306713 ) ) ;
#8564 = VECTOR ( 'NONE', #5496, 1000.000000000000000 ) ;
#8565 = VERTEX_POINT ( 'NONE', #4778 ) ;
#8566 = CARTESIAN_POINT ( 'NONE',  ( 19.90085419568980640, 16.36478119802090703, 11.95042571680015442 ) ) ;
#8567 = SURFACE_STYLE_USAGE ( .BOTH. , #5297 ) ;
#8568 = CARTESIAN_POINT ( 'NONE',  ( 18.64799062861727563, 15.97503555906617123, 11.97707131907271005 ) ) ;
#8569 = CARTESIAN_POINT ( 'NONE',  ( 16.35082997044643704, 18.59891749786092063, 12.19867189564230969 ) ) ;
#8570 = CARTESIAN_POINT ( 'NONE',  ( -25.98076211353311393, 49.89374999904395480, -6.871901078670400231 ) ) ;
#8571 = PRODUCT_DEFINITION ( 'UNKNOWN', '', #2981, #4116 ) ;
#8572 = CARTESIAN_POINT ( 'NONE',  ( -1.035533905932736420, 27.49999999999998934, 14.20312500000000355 ) ) ;
#8573 = DIRECTION ( 'NONE',  ( -0.000000000000000000, -0.000000000000000000, -1.000000000000000000 ) ) ;
#8574 = DIRECTION ( 'NONE',  ( 0.000000000000000000, 0.8660254037844380415, -0.5000000000000012212 ) ) ;
#8575 = ORIENTED_EDGE ( 'NONE', *, *, #10041, .T. ) ;
#8576 = VERTEX_POINT ( 'NONE', #5608 ) ;
#8577 = CARTESIAN_POINT ( 'NONE',  ( 17.86810043078960319, 17.16701444005803268, 12.06109941161078325 ) ) ;
#8578 = DIRECTION ( 'NONE',  ( 0.000000000000000000, 0.000000000000000000, -1.000000000000000000 ) ) ;
#8579 = CARTESIAN_POINT ( 'NONE',  ( 21.41951502703731691, 22.64547864373410135, 12.00579112326941988 ) ) ;
#8580 = CARTESIAN_POINT ( 'NONE',  ( -26.51666049839534622, 52.50626073911683278, -7.000000000000073719 ) ) ;
#8581 = EDGE_CURVE ( 'NONE', #3184, #3474, #10815, .T. ) ;
#8582 = DIRECTION ( 'NONE',  ( 0.000000000000000000, 0.000000000000000000, 1.000000000000000000 ) ) ;
#8583 = CARTESIAN_POINT ( 'NONE',  ( -25.98076211353311393, 54.09374999904395054, -6.871901078670400231 ) ) ;
#8584 = EDGE_CURVE ( 'NONE', #6109, #10330, #3150, .T. ) ;
#8585 = DIRECTION ( 'NONE',  ( 0.000000000000000000, 0.000000000000000000, 1.000000000000000000 ) ) ;
#8586 = FACE_OUTER_BOUND ( 'NONE', #10841, .T. ) ;
#8587 = LINE ( 'NONE', #8702, #9681 ) ;
#8588 = ORIENTED_EDGE ( 'NONE', *, *, #8238, .T. ) ;
#8589 =( NAMED_UNIT ( * ) PLANE_ANGLE_UNIT ( ) SI_UNIT ( $, .RADIAN. ) );
#8590 = CARTESIAN_POINT ( 'NONE',  ( -1.720978244806810498, 31.81455566112594013, 16.06030841526693820 ) ) ;
#8591 = CARTESIAN_POINT ( 'NONE',  ( -26.51666049839534622, 53.11876073720499392, -7.000000000000073719 ) ) ;
#8592 = CARTESIAN_POINT ( 'NONE',  ( -25.17020516978313083, 53.97708333237728340, -3.596074190997380349 ) ) ;
#8593 = VECTOR ( 'NONE', #6753, 1000.000000000000000 ) ;
#8594 = CARTESIAN_POINT ( 'NONE',  ( -25.17020516978313083, 55.43541666571061910, -6.403925809002825709 ) ) ;
#8595 = ADVANCED_FACE ( 'NONE', ( #6533 ), #6464, .F. ) ;
#8596 = LINE ( 'NONE', #1823, #7311 ) ;
#8597 = DIRECTION ( 'NONE',  ( -0.000000000000000000, -0.000000000000000000, 1.000000000000000000 ) ) ;
#8598 = VECTOR ( 'NONE', #3137, 1000.000000000000000 ) ;
#8599 = ORIENTED_EDGE ( 'NONE', *, *, #4908, .F. ) ;
#8600 = AXIS2_PLACEMENT_3D ( 'NONE', #2782, #5278, #2890 ) ;
#8601 = ORIENTED_EDGE ( 'NONE', *, *, #225, .T. ) ;
#8602 = LINE ( 'NONE', #4218, #3622 ) ;
#8603 = EDGE_CURVE ( 'NONE', #1390, #1944, #260, .T. ) ;
#8604 = CARTESIAN_POINT ( 'NONE',  ( -6.259644161404860030E-16, -4.618802153517027165, -3.433295621305388234 ) ) ;
#8605 = DIRECTION ( 'NONE',  ( 6.123233995736766036E-17, 0.000000000000000000, 1.000000000000000000 ) ) ;
#8606 = ORIENTED_EDGE ( 'NONE', *, *, #3495, .F. ) ;
#8607 = CARTESIAN_POINT ( 'NONE',  ( 2.500000000000000000, -2.357898499370432610, 3.252606517456513302E-15 ) ) ;
#8608 = CARTESIAN_POINT ( 'NONE',  ( 1.391697335622810172, 4.043246145443375461, -3.503898532754365913 ) ) ;
#8609 = AXIS2_PLACEMENT_3D ( 'NONE', #10278, #3449, #6771 ) ;
#8610 = CARTESIAN_POINT ( 'NONE',  ( 2.500000000000000000, -2.357898499370432610, 3.252606517456513302E-15 ) ) ;
#8611 = AXIS2_PLACEMENT_3D ( 'NONE', #10131, #8573, #2518 ) ;
#8612 = CONICAL_SURFACE ( 'NONE', #1876, 5.560781378645573980, 1.221730476396046816 ) ;
#8613 = VECTOR ( 'NONE', #3665, 1000.000000000000000 ) ;
#8614 = CARTESIAN_POINT ( 'NONE',  ( 16.98270770525814299, 16.57081904430127395, 11.07189675232624104 ) ) ;
#8615 = EDGE_CURVE ( 'NONE', #6840, #6853, #5755, .T. ) ;
#8616 = CARTESIAN_POINT ( 'NONE',  ( -31.74999999999995737, 0.000000000000000000, 0.000000000000000000 ) ) ;
#8617 = CARTESIAN_POINT ( 'NONE',  ( -25.17020516978313083, 51.17708333237727913, -3.596074190997380349 ) ) ;
#8618 = CIRCLE ( 'NONE', #8798, 4.499999999999999112 ) ;
#8619 = DIRECTION ( 'NONE',  ( -0.000000000000000000, -0.000000000000000000, -1.000000000000000000 ) ) ;
#8620 = ORIENTED_EDGE ( 'NONE', *, *, #4458, .F. ) ;
#8621 = CARTESIAN_POINT ( 'NONE',  ( 0.000000000000000000, 0.000000000000000000, -4.000000000000000000 ) ) ;
#8622 = EDGE_LOOP ( 'NONE', ( #1714, #5987, #5501, #383, #4559 ) ) ;
#8623 = CARTESIAN_POINT ( 'NONE',  ( 2.428085025993350410, 32.52166244231248271, 13.75219158473306535 ) ) ;
#8624 = VECTOR ( 'NONE', #9418, 1000.000000000000000 ) ;
#8625 = ORIENTED_EDGE ( 'NONE', *, *, #8653, .T. ) ;
#8626 = CARTESIAN_POINT ( 'NONE',  ( 22.99351140629659795, 23.33806509665494389, 12.94889058896590583 ) ) ;
#8627 = DIRECTION ( 'NONE',  ( 1.000000000000000000, 0.000000000000000000, 0.000000000000000000 ) ) ;
#8628 = CARTESIAN_POINT ( 'NONE',  ( 17.20991452582289583, 17.73983294248524700, 12.11810441208646338 ) ) ;
#8630 = CARTESIAN_POINT ( 'NONE',  ( -24.35964822603314417, 51.81874999904395196, -5.000000000000103029 ) ) ;
#8629 = VECTOR ( 'NONE', #3303, 1000.000000000000000 ) ;
#8631 = CARTESIAN_POINT ( 'NONE',  ( 1.767766952966372429, 31.76776695296637598, 14.75000000000000355 ) ) ;
#8632 = LINE ( 'NONE', #4188, #6461 ) ;
#8633 = DIRECTION ( 'NONE',  ( -1.000000000000000000, -0.000000000000000000, -0.000000000000000000 ) ) ;
#8634 = ORIENTED_EDGE ( 'NONE', *, *, #8236, .F. ) ;
#8635 = ORIENTED_EDGE ( 'NONE', *, *, #632, .F. ) ;
#8636 = DIRECTION ( 'NONE',  ( 0.000000000000000000, 0.000000000000000000, -1.000000000000000000 ) ) ;
#8637 = FACE_BOUND ( 'NONE', #7003, .T. ) ;
#8638 =( LENGTH_UNIT ( ) NAMED_UNIT ( * ) SI_UNIT ( .MILLI., .METRE. ) );
#8639 = EDGE_CURVE ( 'NONE', #1738, #7809, #4133, .T. ) ;
#8640 = CARTESIAN_POINT ( 'NONE',  ( 1.035533905932737975, 32.50000000000000711, 14.82812500000000355 ) ) ;
#8641 = CARTESIAN_POINT ( 'NONE',  ( 0.000000000000000000, 30.00000000000000000, 2.500000000000000000 ) ) ;
#8642 = CARTESIAN_POINT ( 'NONE',  ( -25.98076211353311393, 55.14374999904394059, -3.128098921329806714 ) ) ;
#8643 = CARTESIAN_POINT ( 'NONE',  ( 26.17691601781025312, 59.99615088301337096, -2.500000000000000000 ) ) ;
#8644 = CARTESIAN_POINT ( 'NONE',  ( -24.98076211353193798, 57.99999999999910472, -3.267949192431741423 ) ) ;
#8645 = CARTESIAN_POINT ( 'NONE',  ( 29.49999999999999289, 14.99999999999984546, -2.500000000000000000 ) ) ;
#8646 = EDGE_LOOP ( 'NONE', ( #5715, #365, #7778, #4947 ) ) ;
#8647 = SURFACE_SIDE_STYLE ('',( #5319 ) ) ;
#8648 = CARTESIAN_POINT ( 'NONE',  ( -2.500000000000007550, 31.03553390593274486, 15.14062500000000355 ) ) ;
#8649 = AXIS2_PLACEMENT_3D ( 'NONE', #4859, #9235, #1418 ) ;
#8650 = AXIS2_PLACEMENT_3D ( 'NONE', #10829, #2441, #8436 ) ;
#8651 = PLANE ( 'NONE',  #9551 ) ;
#8652 = UNCERTAINTY_MEASURE_WITH_UNIT (LENGTH_MEASURE( 1.000000000000000082E-05 ), #10773, 'distance_accuracy_value', 'NONE');
#8653 = EDGE_CURVE ( 'NONE', #10663, #7434, #1139, .T. ) ;
#8654 = CARTESIAN_POINT ( 'NONE',  ( -26.79131905728310059, 55.02708333237728056, -6.403925809002825709 ) ) ;
#8655 = CARTESIAN_POINT ( 'NONE',  ( -25.44486372867087454, 54.95626073911682852, -3.000000000000134559 ) ) ;
#8656 = EDGE_CURVE ( 'NONE', #2953, #4777, #9536, .T. ) ;
#8657 = PLANE ( 'NONE',  #6583 ) ;
#8658 = VECTOR ( 'NONE', #4567, 1000.000000000000000 ) ;
#8659 = AXIS2_PLACEMENT_3D ( 'NONE', #2857, #6227, #4630 ) ;
#8660 = CARTESIAN_POINT ( 'NONE',  ( 25.49999999999999645, -3.999999999999986233, -6.649999999999990585 ) ) ;
#8661 = ORIENTED_EDGE ( 'NONE', *, *, #158, .T. ) ;
#8662 = ORIENTED_EDGE ( 'NONE', *, *, #1583, .T. ) ;
#8663 = CARTESIAN_POINT ( 'NONE',  ( 4.000000000000000000, 2.309401076758497151, -5.000000000000000000 ) ) ;
#8664 = ADVANCED_FACE ( 'NONE', ( #1986 ), #5373, .F. ) ;
#8665 = DIRECTION ( 'NONE',  ( -1.000000000000000000, -0.000000000000000000, -0.000000000000000000 ) ) ;
#8666 = APPLICATION_PROTOCOL_DEFINITION ( 'draft international standard', 'automotive_design', 1998, #7789 ) ;
#8667 = VERTEX_POINT ( 'NONE', #4547 ) ;
#8668 = MECHANICAL_DESIGN_GEOMETRIC_PRESENTATION_REPRESENTATION (  '', ( #6889 ), #1743 ) ;
#8669 = CARTESIAN_POINT ( 'NONE',  ( 3.200000000000000622, 3.202582148906713222, -1.452965002680467910 ) ) ;
#8670 = CARTESIAN_POINT ( 'NONE',  ( 5.076455387921339657, 24.47916666666667140, -2.499999999999998668 ) ) ;
#8671 = EDGE_CURVE ( 'NONE', #2510, #3184, #4943, .T. ) ;
#8672 = EDGE_CURVE ( 'NONE', #6838, #10287, #8921, .T. ) ;
#8673 = CARTESIAN_POINT ( 'NONE',  ( 23.54706165660595829, 18.96431965174070555, 11.95042449705224819 ) ) ;
#8674 = CARTESIAN_POINT ( 'NONE',  ( 29.50000000000000711, 5.000000000000001776, -2.500000000000000000 ) ) ;
#8675 = CARTESIAN_POINT ( 'NONE',  ( -26.79131905728310059, 51.52708333237728056, -6.403925809002825709 ) ) ;
#8676 = AXIS2_PLACEMENT_3D ( 'NONE', #2711, #4491, #248 ) ;
#8677 = LINE ( 'NONE', #10455, #10169 ) ;
#8678 = ORIENTED_EDGE ( 'NONE', *, *, #131, .F. ) ;
#8679 = DIRECTION ( 'NONE',  ( 1.000000000000000000, -0.000000000000000000, -0.000000000000000000 ) ) ;
#8680 = ORIENTED_EDGE ( 'NONE', *, *, #5808, .T. ) ;
#8681 = AXIS2_PLACEMENT_3D ( 'NONE', #8910, #10682, #8132 ) ;
#8682 = CARTESIAN_POINT ( 'NONE',  ( 3.527408190673962274, 28.61642175733934934, 13.51781658473306713 ) ) ;
#8683 = VERTEX_POINT ( 'NONE', #1310 ) ;
#8684 = CARTESIAN_POINT ( 'NONE',  ( 20.15426471261298147, 16.54100339847095213, 11.95042283504686154 ) ) ;
#8685 = DIRECTION ( 'NONE',  ( 0.000000000000000000, 0.000000000000000000, 1.000000000000000000 ) ) ;
#8686 = CARTESIAN_POINT ( 'NONE',  ( 21.90605485701305000, 18.97586566459109392, 12.00579112326941988 ) ) ;
#8687 = CARTESIAN_POINT ( 'NONE',  ( -26.79131905728310059, 51.35208333237728340, -6.403925809002825709 ) ) ;
#8688 = DIRECTION ( 'NONE',  ( 0.000000000000000000, 0.000000000000000000, 1.000000000000000000 ) ) ;
#8689 = CARTESIAN_POINT ( 'NONE',  ( 24.49999999999998934, -3.999999999999983569, 10.00000000000000888 ) ) ;
#8690 = FACE_OUTER_BOUND ( 'NONE', #7605, .T. ) ;
#8691 = ORIENTED_EDGE ( 'NONE', *, *, #6748, .F. ) ;
#8692 = ADVANCED_FACE ( 'NONE', ( #9644 ), #6251, .F. ) ;
#8693 = VERTEX_POINT ( 'NONE', #2038 ) ;
#8694 = DIRECTION ( 'NONE',  ( -1.000000000000000000, 0.000000000000000000, -0.000000000000000000 ) ) ;
#8695 = CARTESIAN_POINT ( 'NONE',  ( 29.50000000000000711, -3.999999999999989786, -7.149999999999991473 ) ) ;
#8696 = FILL_AREA_STYLE ('',( #5311 ) ) ;
#8697 = CARTESIAN_POINT ( 'NONE',  ( 0.000000000000000000, 30.00000000000000000, -23.71320343559643007 ) ) ;
#8698 = CARTESIAN_POINT ( 'NONE',  ( 2.500000000000000000, -1.178949249685213863, 2.042000000000002924 ) ) ;
#8699 = DIRECTION ( 'NONE',  ( 0.000000000000000000, -0.5000000000000011102, -0.8660254037844379305 ) ) ;
#8700 = DIRECTION ( 'NONE',  ( 0.000000000000000000, 1.000000000000000000, 0.000000000000000000 ) ) ;
#8701 = DIRECTION ( 'NONE',  ( 1.000000000000000000, 0.000000000000000000, 0.000000000000000000 ) ) ;
#8702 = CARTESIAN_POINT ( 'NONE',  ( 34.99999999999987210, -3.999999999999989786, 12.14999999999999147 ) ) ;
#8703 = EDGE_LOOP ( 'NONE', ( #8176, #6348, #6558, #10189 ) ) ;
#8704 = CARTESIAN_POINT ( 'NONE',  ( -2.500000000000005773, 29.99999999999999645, 16.46875000000000355 ) ) ;
#8705 = CARTESIAN_POINT ( 'NONE',  ( -1.767766952966370209, 28.23223304703362402, 15.37500000000000355 ) ) ;
#8706 = CARTESIAN_POINT ( 'NONE',  ( 0.2704726383733979667, 0.000000000000000000, 1.650000000000000355 ) ) ;
#8707 = CARTESIAN_POINT ( 'NONE',  ( -24.98076211353312814, 53.72916666475470038, -6.732050807568954909 ) ) ;
#8708 = CARTESIAN_POINT ( 'NONE',  ( 29.50000000000000711, -3.999999999999989786, -4.999999999999999112 ) ) ;
#8709 = CARTESIAN_POINT ( 'NONE',  ( -23.98076211353314235, 55.04166666666652930, -3.845299461620867554 ) ) ;
#8710 = ORIENTED_EDGE ( 'NONE', *, *, #9770, .F. ) ;
#8711 = ORIENTED_EDGE ( 'NONE', *, *, #8653, .F. ) ;
#8712 = PLANE ( 'NONE',  #4870 ) ;
#8713 = EDGE_CURVE ( 'NONE', #6644, #9280, #3432, .T. ) ;
#8714 = DIRECTION ( 'NONE',  ( 0.000000000000000000, 1.000000000000000000, 0.000000000000000000 ) ) ;
#8715 = PRODUCT_CONTEXT ( 'NONE', #8134, 'mechanical' ) ;
#8716 = VERTEX_POINT ( 'NONE', #6145 ) ;
#8717 = DIRECTION ( 'NONE',  ( 0.000000000000000000, 0.5000000000000011102, 0.8660254037844379305 ) ) ;
#8718 = AXIS2_PLACEMENT_3D ( 'NONE', #5478, #8133, #7086 ) ;
#8719 = CARTESIAN_POINT ( 'NONE',  ( 24.30992024302470256, 5.833333333333335702, 2.500000000000000000 ) ) ;
#8720 = CARTESIAN_POINT ( 'NONE',  ( 20.05583492806123758, 17.75628287944761396, 11.00732503135576401 ) ) ;
#8721 = EDGE_CURVE ( 'NONE', #874, #40, #3760, .T. ) ;
#8722 = DIRECTION ( 'NONE',  ( -0.000000000000000000, -1.000000000000000000, -0.000000000000000000 ) ) ;
#8723 = EDGE_CURVE ( 'NONE', #4377, #3105, #10013, .T. ) ;
#8724 = CARTESIAN_POINT ( 'NONE',  ( -27.60187600103308014, 53.68541666571061199, -5.935950539335252074 ) ) ;
#8725 = CIRCLE ( 'NONE', #5359, 3.250000000000000000 ) ;
#8726 = DIRECTION ( 'NONE',  ( -0.000000000000000000, 1.471414886128461471E-15, 1.000000000000000000 ) ) ;
#8727 = ORIENTED_EDGE ( 'NONE', *, *, #8266, .F. ) ;
#8728 = SPHERICAL_SURFACE ( 'NONE', #3865, 3.250000000000000000 ) ;
#8729 = ORIENTED_EDGE ( 'NONE', *, *, #7443, .T. ) ;
#8730 = CARTESIAN_POINT ( 'NONE',  ( -2.527408190673963162, 30.96936468028755840, 12.89281658473306535 ) ) ;
#8731 = EDGE_LOOP ( 'NONE', ( #2011, #172, #5809, #9237, #8885 ) ) ;
#8732 = CARTESIAN_POINT ( 'NONE',  ( 24.14247934234231963, 22.08663129433533001, 12.94889058896630019 ) ) ;
#8733 = DIRECTION ( 'NONE',  ( 0.000000000000000000, 0.000000000000000000, 1.000000000000000000 ) ) ;
#8734 = CARTESIAN_POINT ( 'NONE',  ( 21.25655365073496839, 18.52406763439849513, 12.00579112326941988 ) ) ;
#8735 = CARTESIAN_POINT ( 'NONE',  ( -25.98076211353311393, 55.14374999904394059, -3.128098921329806714 ) ) ;
#8736 = CARTESIAN_POINT ( 'NONE',  ( 29.50000000000000711, -2.999999999999962697, -17.49999999999999645 ) ) ;
#8737 = DIRECTION ( 'NONE',  ( -1.000000000000000000, -6.098637220230963674E-17, -1.156482317317871478E-16 ) ) ;
#8738 = DIRECTION ( 'NONE',  ( 0.000000000000000000, 1.000000000000000000, 0.000000000000000000 ) ) ;
#8739 = VERTEX_POINT ( 'NONE', #8706 ) ;
#8740 = DIRECTION ( 'NONE',  ( 0.000000000000000000, -0.5000000000000011102, -0.8660254037844379305 ) ) ;
#8741 = DIRECTION ( 'NONE',  ( 0.000000000000000000, 0.000000000000000000, 1.000000000000000000 ) ) ;
#8742 = DIRECTION ( 'NONE',  ( 0.000000000000000000, 0.000000000000000000, -1.000000000000000000 ) ) ;
#8743 = VECTOR ( 'NONE', #8929, 1000.000000000000114 ) ;
#8744 = DIRECTION ( 'NONE',  ( -0.000000000000000000, -0.000000000000000000, -1.000000000000000000 ) ) ;
#8745 =( BOUNDED_CURVE ( )  B_SPLINE_CURVE ( 2, ( #2936, #3707, #6312, #3653, #5324, #10488, #2100, #8877, #1261 ),
 .UNSPECIFIED., .F., .F. ) 
 B_SPLINE_CURVE_WITH_KNOTS ( ( 3, 2, 2, 2, 3 ),
 ( 0.5277777777777777901, 0.5370370370370370905, 0.5555555555555555802, 0.5740740740740740700, 0.5833333333333333703 ),
 .UNSPECIFIED. ) 
 CURVE ( )  GEOMETRIC_REPRESENTATION_ITEM ( )  RATIONAL_B_SPLINE_CURVE ( ( 0.9330127018922194093, 0.9330127018922194093, 1.000000000000000000, 0.8660254037844387076, 1.000000000000000000, 0.8660254037844387076, 1.000000000000000000, 0.9330127018922189652, 0.9330127018922194093 ) ) 
 REPRESENTATION_ITEM ( '' )  );
#8746 = CARTESIAN_POINT ( 'NONE',  ( 1.390230914382191596, 4.043987460488659202, -3.502507215260488582 ) ) ;
#8747 = CARTESIAN_POINT ( 'NONE',  ( -27.60187600103308370, 55.66874999904394627, -5.000000000000103029 ) ) ;
#8748 =( NAMED_UNIT ( * ) PLANE_ANGLE_UNIT ( ) SI_UNIT ( $, .RADIAN. ) );
#8749 = CARTESIAN_POINT ( 'NONE',  ( 2.474873734152918558, 32.47487373415292211, 16.00000000000000355 ) ) ;
#8750 = DIRECTION ( 'NONE',  ( 0.000000000000000000, 0.000000000000000000, 1.000000000000000000 ) ) ;
#8751 = ADVANCED_FACE ( 'NONE', ( #1085 ), #8876, .T. ) ;
#8752 = ORIENTED_EDGE ( 'NONE', *, *, #9942, .F. ) ;
#8753 = DIRECTION ( 'NONE',  ( -0.000000000000000000, -0.000000000000000000, 1.000000000000000000 ) ) ;
#8754 = B_SPLINE_CURVE_WITH_KNOTS ( 'NONE', 3,
 ( #9692, #557, #3075, #3955, #6448, #8804 ),
 .UNSPECIFIED., .F., .F.,
 ( 4, 2, 4 ),
 ( 0.000000000000000000, 0.0002095117440854740156, 0.0004190234881709480313 ),
 .UNSPECIFIED. ) ;
#8755 = CARTESIAN_POINT ( 'NONE',  ( 1.767766952966372429, 31.76776695296637598, 14.75000000000000355 ) ) ;
#8756 = DIRECTION ( 'NONE',  ( -0.9876851083892491667, -0.1564548710207423754, 0.000000000000000000 ) ) ;
#8757 = CARTESIAN_POINT ( 'NONE',  ( 34.99999999999987210, -3.999999999999989786, 9.999999999999998224 ) ) ;
#8758 = CARTESIAN_POINT ( 'NONE',  ( 0.2174200650117457945, 2.185595227304829802, -3.214438021527938893 ) ) ;
#8759 = CARTESIAN_POINT ( 'NONE',  ( -24.35964822603314772, 52.05208333237727913, -5.935950539335252074 ) ) ;
#8760 = CARTESIAN_POINT ( 'NONE',  ( 2.000000000000000000, 1.880445160090761061E-16, -1.535500000000000087 ) ) ;
#8761 = CARTESIAN_POINT ( 'NONE',  ( -24.98076211353312814, 54.51666666666653072, -6.732050807568954909 ) ) ;
#8762 = VERTEX_POINT ( 'NONE', #8037 ) ;
#8763 = EDGE_LOOP ( 'NONE', ( #4192, #8752, #7517 ) ) ;
#8764 = CARTESIAN_POINT ( 'NONE',  ( -26.98076211353309972, 54.63333333333319786, -6.732050807568954909 ) ) ;
#8765 = APPLICATION_CONTEXT ( 'automotive_design' ) ;
#8766 = FACE_OUTER_BOUND ( 'NONE', #9915, .T. ) ;
#8767 = CARTESIAN_POINT ( 'NONE',  ( 0.000000000000000000, 0.000000000000000000, 0.000000000000000000 ) ) ;
#8768 = ORIENTED_EDGE ( 'NONE', *, *, #10486, .F. ) ;
#8769 = CIRCLE ( 'NONE', #3804, 2.149999999999990585 ) ;
#8770 = CARTESIAN_POINT ( 'NONE',  ( -3.333333333333332149, -2.694301256218264218, -3.300726591567082036 ) ) ;
#8771 = DIRECTION ( 'NONE',  ( 0.000000000000000000, 8.673617379884032514E-16, 1.000000000000000000 ) ) ;
#8772 = EDGE_CURVE ( 'NONE', #6022, #10302, #2755, .T. ) ;
#8773 = CARTESIAN_POINT ( 'NONE',  ( 18.94282644159813955, 20.01493855567512625, 10.95195840513859231 ) ) ;
#8774 = ORIENTED_EDGE ( 'NONE', *, *, #2830, .F. ) ;
#8775 = CARTESIAN_POINT ( 'NONE',  ( -27.60187600103308014, 51.70208333237727771, -4.064049460664955760 ) ) ;
#8776 = ORIENTED_EDGE ( 'NONE', *, *, #7096, .T. ) ;
#8777 = DIRECTION ( 'NONE',  ( 0.000000000000000000, 1.000000000000000000, 0.000000000000000000 ) ) ;
#8778 = EDGE_LOOP ( 'NONE', ( #5831, #9610, #9955, #6061 ) ) ;
#8779 = CARTESIAN_POINT ( 'NONE',  ( 0.06616922564517943584, 27.49999999999998934, 13.28344158473306713 ) ) ;
#8780 = VECTOR ( 'NONE', #8543, 1000.000000000000000 ) ;
#8781 = ORIENTED_EDGE ( 'NONE', *, *, #2559, .F. ) ;
#8782 = CARTESIAN_POINT ( 'NONE',  ( 22.86591953417209666, 18.42728137938113875, 11.95042449705224819 ) ) ;
#8783 = SHAPE_REPRESENTATION_RELATIONSHIP ( 'NONE' , 'NONE' ,  #5283, #3752 ) ;
#8784 = AXIS2_PLACEMENT_3D ( 'NONE', #9715, #2052, #2843 ) ;
#8785 = EDGE_CURVE ( 'NONE', #8489, #276, #1148, .T. ) ;
#8786 = CARTESIAN_POINT ( 'NONE',  ( 18.88912242859132107, 19.99746927611068870, 11.95042449705224819 ) ) ;
#8787 = EDGE_CURVE ( 'NONE', #6331, #9431, #424, .T. ) ;
#8788 = CIRCLE ( 'NONE', #4168, 2.149999999999988809 ) ;
#8789 = CARTESIAN_POINT ( 'NONE',  ( 16.70557116688603472, 16.82996273904517182, 13.10128505860060066 ) ) ;
#8790 = CARTESIAN_POINT ( 'NONE',  ( -24.35964822603314772, 53.97708333237728340, -5.935950539335252074 ) ) ;
#8791 = SURFACE_STYLE_FILL_AREA ( #10466 ) ;
#8792 = LINE ( 'NONE', #3737, #269 ) ;
#8793 = CARTESIAN_POINT ( 'NONE',  ( 26.25045812061784289, 0.000000000000000000, 10.00000000000000178 ) ) ;
#8794 = ORIENTED_EDGE ( 'NONE', *, *, #10008, .F. ) ;
#8795 = ORIENTED_EDGE ( 'NONE', *, *, #8990, .F. ) ;
#8796 = CARTESIAN_POINT ( 'NONE',  ( 15.88045857259785087, 19.06928889570832197, 12.24278471274156388 ) ) ;
#8797 = EDGE_CURVE ( 'NONE', #2763, #1093, #683, .T. ) ;
#8798 = AXIS2_PLACEMENT_3D ( 'NONE', #9795, #2184, #2242 ) ;
#8799 = CARTESIAN_POINT ( 'NONE',  ( 0.000000000000000000, 0.000000000000000000, 0.000000000000000000 ) ) ;
#8800 =( BOUNDED_SURFACE ( )  B_SPLINE_SURFACE ( 3, 2, ( 
 ( #4924, #8298, #8920 ),
 ( #1366, #4765, #8143 ),
 ( #3086, #6460, #5648 ),
 ( #5912, #8353, #3305 ),
 ( #5033, #6686, #2650 ),
 ( #732, #1809, #16 ) ),
 .UNSPECIFIED., .F., .F., .F. ) 
 B_SPLINE_SURFACE_WITH_KNOTS ( ( 4, 2, 4 ),
 ( 3, 3 ),
 ( 0.02027752710269158445, 0.02273781595091097299, 0.02519810479913036153 ),
 ( 0.000000000000000000, 1.000000000000000000 ),
 .UNSPECIFIED. ) 
 GEOMETRIC_REPRESENTATION_ITEM ( )  RATIONAL_B_SPLINE_SURFACE ( (
 ( 1.000000000000000000, 0.8047781431712808242, 1.000000000000000000),
 ( 1.000000000000000000, 0.8123773247083928561, 1.000000000000000000),
 ( 1.000000000000000000, 0.8190670192154906326, 1.000000000000000000),
 ( 1.000000000000000000, 0.8192353552912178261, 1.000000000000000000),
 ( 1.000000000000000000, 0.8126132098226825917, 1.000000000000000000),
 ( 1.000000000000000000, 0.8047712465856394770, 1.000000000000000000) ) ) 
 REPRESENTATION_ITEM ( '' )  SURFACE ( )  );
#8801 = CARTESIAN_POINT ( 'NONE',  ( -25.98076211353311393, 50.02499999999987068, -3.000000000000132783 ) ) ;
#8802 = AXIS2_PLACEMENT_3D ( 'NONE', #10191, #4080, #5911 ) ;
#8803 = DIRECTION ( 'NONE',  ( 1.000000000000000000, 0.000000000000000000, 0.000000000000000000 ) ) ;
#8804 = CARTESIAN_POINT ( 'NONE',  ( -6.473970235329672780E-16, -4.862606272033106691, -3.745885042887442395 ) ) ;
#8805 = CARTESIAN_POINT ( 'NONE',  ( -25.98076211353311749, 56.99999999999884182, -7.000000000000094147 ) ) ;
#8806 = LINE ( 'NONE', #1249, #2263 ) ;
#8807 = EDGE_CURVE ( 'NONE', #7218, #9728, #9031, .T. ) ;
#8808 = EDGE_CURVE ( 'NONE', #2222, #1168, #2578, .T. ) ;
#8809 = DIRECTION ( 'NONE',  ( 0.000000000000000000, -0.4999999999999993894, 0.8660254037844389297 ) ) ;
#8810 = CARTESIAN_POINT ( 'NONE',  ( 1.449747468305836673, 26.49999999999999289, 15.60937500000000711 ) ) ;
#8811 = DIRECTION ( 'NONE',  ( -1.000000000000000000, -0.000000000000000000, -0.000000000000000000 ) ) ;
#8812 = ORIENTED_EDGE ( 'NONE', *, *, #2748, .F. ) ;
#8813 = FACE_BOUND ( 'NONE', #877, .T. ) ;
#8814 = CIRCLE ( 'NONE', #9699, 2.500000000000000888 ) ;
#8815 = CARTESIAN_POINT ( 'NONE',  ( 1.101703131577913553, 32.47259180932605460, 15.82593341526694353 ) ) ;
#8816 = CARTESIAN_POINT ( 'NONE',  ( -26.51666049839534978, 53.40623925897106972, -3.000000000000133227 ) ) ;
#8817 = CARTESIAN_POINT ( 'NONE',  ( 19.05040816462259556, 17.06282649731835122, 12.00984920396035172 ) ) ;
#8818 =( BOUNDED_CURVE ( )  B_SPLINE_CURVE ( 2, ( #4433, #8580, #964, #4371, #7815, #7756, #137, #3537, #5257 ),
 .UNSPECIFIED., .F., .F. ) 
 B_SPLINE_CURVE_WITH_KNOTS ( ( 3, 2, 2, 2, 3 ),
 ( 0.4722222222222222099, 0.4814814814814814548, 0.5000000000000000000, 0.5185185185185184897, 0.5277777777777777901 ),
 .UNSPECIFIED. ) 
 CURVE ( )  GEOMETRIC_REPRESENTATION_ITEM ( )  RATIONAL_B_SPLINE_CURVE ( ( 0.9330127018922194093, 0.9330127018922194093, 1.000000000000000000, 0.8660254037844387076, 1.000000000000000000, 0.8660254037844387076, 1.000000000000000000, 0.9330127018922194093, 0.9330127018922194093 ) ) 
 REPRESENTATION_ITEM ( '' )  );
#8819 = CARTESIAN_POINT ( 'NONE',  ( -26.24705249213157288, 57.02715675374773951, -6.986049842788033537 ) ) ;
#8820 = CARTESIAN_POINT ( 'NONE',  ( 4.000000000000000000, 3.500000000000000000, 0.000000000000000000 ) ) ;
#8821 = CARTESIAN_POINT ( 'NONE',  ( 5.076455387921339657, 24.47916666666667140, 2.500000000000000000 ) ) ;
#8822 = CARTESIAN_POINT ( 'NONE',  ( -25.17020516978313083, 52.57708333237728482, -3.596074190997380349 ) ) ;
#8823 = DIRECTION ( 'NONE',  ( 1.000000000000000000, -0.000000000000000000, -0.000000000000000000 ) ) ;
#8824 = CARTESIAN_POINT ( 'NONE',  ( -23.98076211353314235, 55.09999999999986642, -5.000000000000103029 ) ) ;
#8825 = ORIENTED_EDGE ( 'NONE', *, *, #10223, .F. ) ;
#8826 = PRESENTATION_LAYER_ASSIGNMENT (  '', '', ( #7393 ) ) ;
#8827 = ORIENTED_EDGE ( 'NONE', *, *, #10990, .T. ) ;
#8828 = CARTESIAN_POINT ( 'NONE',  ( 2.500000000000000888, 3.061616997868384127E-16, -4.974599999999998801 ) ) ;
#8829 = EDGE_CURVE ( 'NONE', #5586, #9268, #4926, .T. ) ;
#8830 = CYLINDRICAL_SURFACE ( 'NONE', #10903, 4.000000000000599520 ) ;
#8831 = ITEM_DEFINED_TRANSFORMATION ( 'NONE', 'NONE', #5801,  #308 ) ;
#8832 = ORIENTED_EDGE ( 'NONE', *, *, #1117, .F. ) ;
#8833 = CARTESIAN_POINT ( 'NONE',  ( -31.74999999999995737, 0.000000000000000000, 3.500000000000000000 ) ) ;
#8834 = CARTESIAN_POINT ( 'NONE',  ( 1.567478505476134606E-15, 4.618802153517012066, -3.433295621305382905 ) ) ;
#8835 = CIRCLE ( 'NONE', #4579, 7.500000000000000000 ) ;
#8836 = CARTESIAN_POINT ( 'NONE',  ( 17.82405332881840110, 17.21173750719964346, 11.06307126761931769 ) ) ;
#8837 = ORIENTED_EDGE ( 'NONE', *, *, #7878, .F. ) ;
#8838 = CARTESIAN_POINT ( 'NONE',  ( -25.98076211353311393, 54.61874999904394912, -3.128098921329806714 ) ) ;
#8839 = ORIENTED_EDGE ( 'NONE', *, *, #2088, .T. ) ;
#8840 = ORIENTED_EDGE ( 'NONE', *, *, #1888, .T. ) ;
#8841 = AXIS2_PLACEMENT_3D ( 'NONE', #3343, #10120, #171 ) ;
#8842 =( GEOMETRIC_REPRESENTATION_CONTEXT ( 3 ) GLOBAL_UNCERTAINTY_ASSIGNED_CONTEXT ( ( #198 ) ) GLOBAL_UNIT_ASSIGNED_CONTEXT ( ( #3270, #3217, #9995 ) ) REPRESENTATION_CONTEXT ( 'NONE', 'WORKASPACE' ) );
#8843 = CARTESIAN_POINT ( 'NONE',  ( -1.720978244806803170, 28.18544433887405987, 13.12719158473306535 ) ) ;
#8844 = ORIENTED_EDGE ( 'NONE', *, *, #8938, .F. ) ;
#8845 = ADVANCED_FACE ( 'NONE', ( #6570 ), #7716, .F. ) ;
#8846 = COLOUR_RGB ( '', 0.66274510, 0.83137255, 0.94901961) ;
#8847 = CARTESIAN_POINT ( 'NONE',  ( 18.94282644159813955, 20.01493855567512625, 10.95195840513859231 ) ) ;
#8848 = SURFACE_STYLE_USAGE ( .BOTH. , #7072 ) ;
#8849 = LINE ( 'NONE', #9510, #10960 ) ;
#8850 = CARTESIAN_POINT ( 'NONE',  ( 17.83714238635922911, 17.16560587574106123, 13.06440897074317853 ) ) ;
#8851 = CARTESIAN_POINT ( 'NONE',  ( -26.98076211353309972, 49.73333333333319928, -6.732050807568954909 ) ) ;
#8852 = AXIS2_PLACEMENT_3D ( 'NONE', #454, #4804, #2139 ) ;
#8853 = DIRECTION ( 'NONE',  ( -1.000000000000000000, -0.000000000000000000, -0.000000000000000000 ) ) ;
#8854 = CARTESIAN_POINT ( 'NONE',  ( -25.98076211353311393, 50.28749999808804461, -7.000000000000073719 ) ) ;
#8855 = DIRECTION ( 'NONE',  ( -0.000000000000000000, -0.000000000000000000, -1.000000000000000000 ) ) ;
#8856 = ORIENTED_EDGE ( 'NONE', *, *, #981, .T. ) ;
#8857 = EDGE_CURVE ( 'NONE', #516, #7151, #7353, .T. ) ;
#8858 = ORIENTED_EDGE ( 'NONE', *, *, #10214, .T. ) ;
#8859 = EDGE_CURVE ( 'NONE', #7739, #7929, #570, .T. ) ;
#8860 = ADVANCED_FACE ( 'NONE', ( #8978 ), #963, .T. ) ;
#8861 = CARTESIAN_POINT ( 'NONE',  ( 19.08509339279509831, 17.01892842213374735, 13.00828316275149099 ) ) ;
#8862 = DIRECTION ( 'NONE',  ( 0.000000000000000000, 1.000000000000000000, 0.000000000000000000 ) ) ;
#8863 = CARTESIAN_POINT ( 'NONE',  ( -25.44486372867087454, 50.05626073911682994, -3.000000000000132339 ) ) ;
#8864 = DIRECTION ( 'NONE',  ( -0.5000000000000051070, 0.000000000000000000, 0.8660254037844355990 ) ) ;
#8865 = CARTESIAN_POINT ( 'NONE',  ( 21.55579831881754416, 20.86490736922957367, 14.50000000000000000 ) ) ;
#8866 = FACE_OUTER_BOUND ( 'NONE', #594, .T. ) ;
#8867 =( NAMED_UNIT ( * ) PLANE_ANGLE_UNIT ( ) SI_UNIT ( $, .RADIAN. ) );
#8868 = DIRECTION ( 'NONE',  ( 0.000000000000000000, -0.000000000000000000, 1.000000000000000000 ) ) ;
#8869 = CARTESIAN_POINT ( 'NONE',  ( 2.474873734152918558, 32.47487373415292211, 13.50000000000000355 ) ) ;
#8870 = CARTESIAN_POINT ( 'NONE',  ( -31.74999999999995737, 0.000000000000000000, 0.000000000000000000 ) ) ;
#8871 = EDGE_CURVE ( 'NONE', #4305, #3617, #8299, .T. ) ;
#8872 = VERTEX_POINT ( 'NONE', #1422 ) ;
#8873 = EDGE_CURVE ( 'NONE', #4861, #9687, #6413, .T. ) ;
#8874 = CARTESIAN_POINT ( 'NONE',  ( 3.472591809326051937, 28.48408330604899419, 16.76343341526694175 ) ) ;
#8875 = FACE_OUTER_BOUND ( 'NONE', #479, .T. ) ;
#8876 = PLANE ( 'NONE',  #6631 ) ;
#8877 = CARTESIAN_POINT ( 'NONE',  ( -25.44486372867087809, 53.14373926088290290, -7.000000000000075495 ) ) ;
#8878 = CARTESIAN_POINT ( 'NONE',  ( -4.141042297810615835, 2.227970268150415656, -3.687027686973619822 ) ) ;
#8879 = CARTESIAN_POINT ( 'NONE',  ( -26.79131905728310059, 52.22708333237727629, -6.403925809002825709 ) ) ;
#8880 = CARTESIAN_POINT ( 'NONE',  ( 5.384454397937118664, 0.000000000000000000, -5.000000000000000000 ) ) ;
#8881 = DIRECTION ( 'NONE',  ( -1.000000000000000000, -0.000000000000000000, -0.000000000000000000 ) ) ;
#8882 = EDGE_LOOP ( 'NONE', ( #4467, #6682, #6151, #7723 ) ) ;
#8883 = CARTESIAN_POINT ( 'NONE',  ( -24.98076211353313170, 50.69583333142136183, -3.267949192431250705 ) ) ;
#8884 = CONTEXT_DEPENDENT_SHAPE_REPRESENTATION ( #5859, #9540 ) ;
#8885 = ORIENTED_EDGE ( 'NONE', *, *, #6407, .T. ) ;
#8886 = DIRECTION ( 'NONE',  ( 0.000000000000000000, 0.000000000000000000, 1.000000000000000000 ) ) ;
#8887 = CARTESIAN_POINT ( 'NONE',  ( 19.48730207459019326, 19.05393922246431870, 11.95042449705224996 ) ) ;
#8888 = CARTESIAN_POINT ( 'NONE',  ( 19.17195227357822773, 19.49818538049391492, 10.95195840513741636 ) ) ;
#8889 = ORIENTED_EDGE ( 'NONE', *, *, #10906, .T. ) ;
#8890 = CARTESIAN_POINT ( 'NONE',  ( -27.60187600103308014, 52.28541666571061342, -5.935950539335252074 ) ) ;
#8892 = ORIENTED_EDGE ( 'NONE', *, *, #6469, .F. ) ;
#8891 = ADVANCED_FACE ( 'NONE', ( #2356 ), #5746, .T. ) ;
#8893 = DIRECTION ( 'NONE',  ( 0.000000000000000000, 1.000000000000000000, 0.000000000000000000 ) ) ;
#8894 = VERTEX_POINT ( 'NONE', #9076 ) ;
#8895 = CARTESIAN_POINT ( 'NONE',  ( 2.500000000000006661, 30.06616922564517580, 14.84594158473306713 ) ) ;
#8896 = EDGE_LOOP ( 'NONE', ( #7783, #6139, #10679, #2277 ) ) ;
#8897 = CARTESIAN_POINT ( 'NONE',  ( 21.79510105275299026, 17.74985623046760708, 10.95195840513859231 ) ) ;
#8898 = CARTESIAN_POINT ( 'NONE',  ( 1.360585162435110629, -4.061296242128317857, -3.505054077164905024 ) ) ;
#8899 = CARTESIAN_POINT ( 'NONE',  ( 20.39832466968983837, 22.29813831026750393, 13.00425721518307753 ) ) ;
#8900 = AXIS2_PLACEMENT_3D ( 'NONE', #5789, #4013, #3956 ) ;
#8901 = LINE ( 'NONE', #230, #2114 ) ;
#8902 = DIRECTION ( 'NONE',  ( 0.9396926207859138680, 1.150791560227856926E-16, -0.3420201433256536139 ) ) ;
#8903 = CARTESIAN_POINT ( 'NONE',  ( 29.49999999999999645, -3.999999999999993339, -4.999999999999995559 ) ) ;
#8904 = VERTEX_POINT ( 'NONE', #520 ) ;
#8905 = EDGE_LOOP ( 'NONE', ( #1712, #5305, #435, #10108 ) ) ;
#8906 = CARTESIAN_POINT ( 'NONE',  ( 23.31827848602400621, 20.57738196266585362, 12.00579112326941988 ) ) ;
#8907 = DIRECTION ( 'NONE',  ( -0.000000000000000000, -0.000000000000000000, -1.000000000000000000 ) ) ;
#8908 = DIRECTION ( 'NONE',  ( 1.000000000000000000, 0.000000000000000000, 0.000000000000000000 ) ) ;
#8909 = CARTESIAN_POINT ( 'NONE',  ( -26.24619511045171194, 58.97315198882180454, -3.013802259003559580 ) ) ;
#8910 = CARTESIAN_POINT ( 'NONE',  ( 25.71106610644839208, 53.49999999999983658, 10.00000000000000178 ) ) ;
#8911 = VECTOR ( 'NONE', #10808, 1000.000000000000000 ) ;
#8912 = CARTESIAN_POINT ( 'NONE',  ( -25.00808978981783781, 57.73360806846572757, -6.748470692696331596 ) ) ;
#8913 = DIRECTION ( 'NONE',  ( -0.000000000000000000, -0.000000000000000000, -1.000000000000000000 ) ) ;
#8914 = EDGE_CURVE ( 'NONE', #10270, #6331, #1238, .T. ) ;
#8915 = CARTESIAN_POINT ( 'NONE',  ( -3.527408190673961386, 28.61642175733934224, 16.29468341526694530 ) ) ;
#8916 = CARTESIAN_POINT ( 'NONE',  ( -25.98076211353311393, 49.49999999999986500, -5.000000000000103029 ) ) ;
#8917 = ORIENTED_EDGE ( 'NONE', *, *, #10884, .T. ) ;
#8918 = CARTESIAN_POINT ( 'NONE',  ( -2.527408190673963162, 29.03063531971243094, 15.04468341526694175 ) ) ;
#8919 = AXIS2_PLACEMENT_3D ( 'NONE', #6834, #9499, #50 ) ;
#8920 = CARTESIAN_POINT ( 'NONE',  ( -4.211399284164270895, 2.459729995988205964, -3.751162237960538715 ) ) ;
#8921 = LINE ( 'NONE', #6311, #8063 ) ;
#8922 = DIRECTION ( 'NONE',  ( -0.7071067811865306973, 0.000000000000000000, 0.7071067811865643371 ) ) ;
#8923 = EDGE_CURVE ( 'NONE', #6926, #3160, #2962, .T. ) ;
#8924 = CARTESIAN_POINT ( 'NONE',  ( -25.98076211353311393, 51.42499999999986926, -3.000000000000132339 ) ) ;
#8925 = CARTESIAN_POINT ( 'NONE',  ( -25.17020516978313083, 53.27708333237728056, -3.596074190997380349 ) ) ;
#8926 = DIRECTION ( 'NONE',  ( 1.000000000000000000, -0.000000000000000000, 1.156482317317871478E-16 ) ) ;
#8927 = CARTESIAN_POINT ( 'NONE',  ( -2.756197834950067094, -3.027510591568735254, -3.223146290109809797 ) ) ;
#8928 = EDGE_LOOP ( 'NONE', ( #7438, #9769 ) ) ;
#8929 = DIRECTION ( 'NONE',  ( 0.000000000000000000, -0.5000000000000011102, -0.8660254037844379305 ) ) ;
#8930 = CARTESIAN_POINT ( 'NONE',  ( -0.3198814748697807464, -4.434118497892185040, -0.3507732604232532969 ) ) ;
#8931 = CONTEXT_DEPENDENT_SHAPE_REPRESENTATION ( #1896, #7772 ) ;
#8932 = VERTEX_POINT ( 'NONE', #1810 ) ;
#8933 = DIRECTION ( 'NONE',  ( 0.000000000000000000, 1.000000000000000000, 0.000000000000000000 ) ) ;
#8934 = EDGE_CURVE ( 'NONE', #3990, #4107, #3809, .T. ) ;
#8935 = CARTESIAN_POINT ( 'NONE',  ( -24.35964822603314417, 51.11874999904394912, -5.000000000000103029 ) ) ;
#8936 = CARTESIAN_POINT ( 'NONE',  ( 17.16312581766332457, 17.78662165064481471, 11.12029599681952519 ) ) ;
#8937 = VERTEX_POINT ( 'NONE', #5858 ) ;
#8938 = EDGE_CURVE ( 'NONE', #8693, #3385, #1638, .T. ) ;
#8939 = DIRECTION ( 'NONE',  ( 0.000000000000000000, 1.000000000000000000, -1.224646799147353207E-16 ) ) ;
#8940 = AXIS2_PLACEMENT_3D ( 'NONE', #10934, #5222, #1657 ) ;
#8941 = VERTEX_POINT ( 'NONE', #2022 ) ;
#8942 = CYLINDRICAL_SURFACE ( 'NONE', #8405, 1.999999999999971356 ) ;
#8943 = ORIENTED_EDGE ( 'NONE', *, *, #623, .F. ) ;
#8944 = CARTESIAN_POINT ( 'NONE',  ( -1.767766952966375094, 31.76776695296636888, 15.06250000000000355 ) ) ;
#8945 = ORIENTED_EDGE ( 'NONE', *, *, #409, .T. ) ;
#8946 = CARTESIAN_POINT ( 'NONE',  ( 16.30404126228686579, 18.64570620602049189, 11.20086348037537327 ) ) ;
#8947 = FILL_AREA_STYLE ('',( #4629 ) ) ;
#8948 = CONICAL_SURFACE ( 'NONE', #3464, 3.499999999999999556, 1.047197551196603849 ) ;
#8949 = EDGE_CURVE ( 'NONE', #6902, #3819, #7343, .T. ) ;
#8950 = PLANE ( 'NONE',  #5636 ) ;
#8951 = CARTESIAN_POINT ( 'NONE',  ( 22.48167088160742821, 22.45759571798082987, 13.00425721518307753 ) ) ;
#8952 = CARTESIAN_POINT ( 'NONE',  ( -25.98076211353311393, 53.08749999808803466, -7.309401076758571314 ) ) ;
#8953 = PRESENTATION_LAYER_ASSIGNMENT (  '', '', ( #3271 ) ) ;
#8954 = CARTESIAN_POINT ( 'NONE',  ( 34.89259351528887976, 2.743407123163641437, -3.513512538347001612 ) ) ;
#8955 = DIRECTION ( 'NONE',  ( 0.000000000000000000, 0.000000000000000000, 1.000000000000000000 ) ) ;
#8956 = ORIENTED_EDGE ( 'NONE', *, *, #6774, .T. ) ;
#8957 = CLOSED_SHELL ( 'NONE', ( #7297, #3382, #7477, #4792, #4886, #8517, #6214, #4254, #7358, #5877, #8071, #8178, #3070, #2964, #4852, #3664, #7350, #6895, #4315, #7226, #4548, #7997, #7989, #7598, #2527, #6380, #6868, #902, #2613, #3025, #10853, #5403, #9956 ) ) ;
#8958 = CIRCLE ( 'NONE', #5592, 34.99999999999999289 ) ;
#8959 = ORIENTED_EDGE ( 'NONE', *, *, #1599, .T. ) ;
#8960 = CARTESIAN_POINT ( 'NONE',  ( 20.08745147943499987, 17.71083118005251933, 12.00579112326941988 ) ) ;
#8961 = VECTOR ( 'NONE', #9438, 1000.000000000000114 ) ;
#8962 = CARTESIAN_POINT ( 'NONE',  ( -9.899505063546603365E-15, 2.000000000000000000, 15.49999999999998046 ) ) ;
#8963 = AXIS2_PLACEMENT_3D ( 'NONE', #9788, #7232, #9901 ) ;
#8964 = CARTESIAN_POINT ( 'NONE',  ( -1.524659305057740610E-17, 0.3418418480469876952, 3.499999999999999556 ) ) ;
#8966 = FACE_OUTER_BOUND ( 'NONE', #8437, .T. ) ;
#8965 = CIRCLE ( 'NONE', #6674, 3.500000000000591971 ) ;
#8967 = TOROIDAL_SURFACE ( 'NONE', #5076, 2.200000000000001066, 0.2000000000000000111 ) ;
#8968 = CARTESIAN_POINT ( 'NONE',  ( 1.515916693951011140, 26.52740819067395250, 13.36156658473306535 ) ) ;
#8969 = CARTESIAN_POINT ( 'NONE',  ( 2.550604951803072673, 0.000000000000000000, 0.000000000000000000 ) ) ;
#8970 = UNCERTAINTY_MEASURE_WITH_UNIT (LENGTH_MEASURE( 1.000000000000000082E-05 ), #9737, 'distance_accuracy_value', 'NONE');
#8971 = EDGE_LOOP ( 'NONE', ( #7493, #928, #5955 ) ) ;
#8972 = CARTESIAN_POINT ( 'NONE',  ( -6.663765011382338240E-15, -3.375361811986485439, 1.153701847711662287 ) ) ;
#8973 = MANIFOLD_SOLID_BREP ( 'M4 Tapped Hole2', #4708 ) ;
#8974 = CARTESIAN_POINT ( 'NONE',  ( -2.472591809326051937, 31.10170313157791000, 17.38843341526693820 ) ) ;
#8975 = VECTOR ( 'NONE', #1026, 1000.000000000000000 ) ;
#8976 = DIRECTION ( 'NONE',  ( -0.000000000000000000, 0.000000000000000000, 1.000000000000000000 ) ) ;
#8977 = ADVANCED_FACE ( 'NONE', ( #6238 ), #10581, .T. ) ;
#8978 = FACE_OUTER_BOUND ( 'NONE', #4157, .T. ) ;
#8979 = FACE_OUTER_BOUND ( 'NONE', #4911, .T. ) ;
#8980 = CARTESIAN_POINT ( 'NONE',  ( -0.6640947660597427138, 4.471078309994878985, -3.602146406945963442 ) ) ;
#8981 = CARTESIAN_POINT ( 'NONE',  ( -25.98076211353311393, 52.86874999904393491, -6.871901078670400231 ) ) ;
#8982 = CARTESIAN_POINT ( 'NONE',  ( 1.828356344711641102, 3.563200125723180900, -5.433716356636336675E-16 ) ) ;
#8983 = CARTESIAN_POINT ( 'NONE',  ( 4.750000000000000888, 0.000000000000000000, 0.000000000000000000 ) ) ;
#8984 = ORIENTED_EDGE ( 'NONE', *, *, #6832, .F. ) ;
#8985 = CARTESIAN_POINT ( 'NONE',  ( 0.000000000000000000, 0.000000000000000000, 0.000000000000000000 ) ) ;
#8986 = PRODUCT_DEFINITION ( 'UNKNOWN', '', #5630, #2457 ) ;
#8987 = DIRECTION ( 'NONE',  ( 0.000000000000000000, 0.000000000000000000, 1.000000000000000000 ) ) ;
#8988 = EDGE_CURVE ( 'NONE', #10050, #3990, #7740, .T. ) ;
#8989 = VERTEX_POINT ( 'NONE', #4432 ) ;
#8990 = EDGE_CURVE ( 'NONE', #5059, #6778, #6111, .T. ) ;
#8991 = CARTESIAN_POINT ( 'NONE',  ( -24.35964822603314772, 51.93541666571061199, -4.064049460664953983 ) ) ;
#8992 = VECTOR ( 'NONE', #7182, 1000.000000000000000 ) ;
#8993 = CARTESIAN_POINT ( 'NONE',  ( -26.79131905728310059, 51.35208333237728340, -6.403925809002825709 ) ) ;
#8994 = CARTESIAN_POINT ( 'NONE',  ( 16.74199038346592872, 18.20775708483950694, 12.16198771834549497 ) ) ;
#8995 =( GEOMETRIC_REPRESENTATION_CONTEXT ( 3 ) GLOBAL_UNCERTAINTY_ASSIGNED_CONTEXT ( ( #8652 ) ) GLOBAL_UNIT_ASSIGNED_CONTEXT ( ( #10773, #5936, #9213 ) ) REPRESENTATION_CONTEXT ( 'NONE', 'WORKASPACE' ) );
#8996 = ORIENTED_EDGE ( 'NONE', *, *, #2943, .F. ) ;
#8997 = CARTESIAN_POINT ( 'NONE',  ( -25.17020516978313083, 55.61041666571061626, -6.403925809002825709 ) ) ;
#8998 = ADVANCED_FACE ( 'NONE', ( #7814 ), #296, .F. ) ;
#8999 = ORIENTED_EDGE ( 'NONE', *, *, #4342, .T. ) ;
#9000 = LINE ( 'NONE', #9940, #10388 ) ;
#9001 = ORIENTED_EDGE ( 'NONE', *, *, #3510, .F. ) ;
#9002 = DIRECTION ( 'NONE',  ( 1.000000000000000000, 0.000000000000000000, 0.000000000000000000 ) ) ;
#9003 =( LENGTH_UNIT ( ) NAMED_UNIT ( * ) SI_UNIT ( .MILLI., .METRE. ) );
#9004 = EDGE_LOOP ( 'NONE', ( #1780, #8510, #4789, #8620 ) ) ;
#9006 = CARTESIAN_POINT ( 'NONE',  ( 19.32754978430113368, 16.15626933694376888, 10.95875375162450638 ) ) ;
#9005 = AXIS2_PLACEMENT_3D ( 'NONE', #4920, #680, #10905 ) ;
#9007 = VECTOR ( 'NONE', #9733, 1000.000000000000000 ) ;
#9008 =( NAMED_UNIT ( * ) PLANE_ANGLE_UNIT ( ) SI_UNIT ( $, .RADIAN. ) );
#9009 = CARTESIAN_POINT ( 'NONE',  ( 2.000000000000000000, 0.8865213383406680414, -1.535500000000000975 ) ) ;
#9010 = CARTESIAN_POINT ( 'NONE',  ( 20.50876875457641546, 17.93645829877244680, 13.00425721518307576 ) ) ;
#9011 = CARTESIAN_POINT ( 'NONE',  ( -26.98076211353309972, 53.14583333142136468, -6.732050807568954909 ) ) ;
#9012 = CIRCLE ( 'NONE', #315, 4.000000000000600409 ) ;
#9013 = STYLED_ITEM ( 'NONE', ( #9216 ), #6261 ) ;
#9014 = CARTESIAN_POINT ( 'NONE',  ( -25.98076211353311393, 53.78749999808803040, -7.000000000000072831 ) ) ;
#9015 = CARTESIAN_POINT ( 'NONE',  ( 3.319999999999999840, 0.000000000000000000, 0.000000000000000000 ) ) ;
#9016 = EDGE_LOOP ( 'NONE', ( #1283, #3002, #2696, #8551 ) ) ;
#9017 = VERTEX_POINT ( 'NONE', #6291 ) ;
#9018 = CARTESIAN_POINT ( 'NONE',  ( 18.65992412991285221, 16.93717640447601269, 13.02011930655217675 ) ) ;
#9019 = STYLED_ITEM ( 'NONE', ( #7544 ), #5559 ) ;
#9020 =( GEOMETRIC_REPRESENTATION_CONTEXT ( 3 ) GLOBAL_UNCERTAINTY_ASSIGNED_CONTEXT ( ( #2591 ) ) GLOBAL_UNIT_ASSIGNED_CONTEXT ( ( #2637, #7686, #2740 ) ) REPRESENTATION_CONTEXT ( 'NONE', 'WORKASPACE' ) );
#9021 = FACE_OUTER_BOUND ( 'NONE', #3887, .T. ) ;
#9022 = CARTESIAN_POINT ( 'NONE',  ( -27.98076211353308196, 56.08556087358027753, -4.543513051204862485 ) ) ;
#9023 = CARTESIAN_POINT ( 'NONE',  ( 2.000000000000000000, -1.773042676681341856, 2.276824562219559311E-15 ) ) ;
#9024 = CARTESIAN_POINT ( 'NONE',  ( -1.720978244806803170, 28.18544433887405987, 13.12719158473306535 ) ) ;
#9025 = CARTESIAN_POINT ( 'NONE',  ( 0.000000000000000000, 0.000000000000000000, -2.500000000000000000 ) ) ;
#9026 = DIRECTION ( 'NONE',  ( -1.000000000000000000, -6.098637220230964906E-17, 0.000000000000000000 ) ) ;
#9027 = CARTESIAN_POINT ( 'NONE',  ( -26.98076211353309972, 55.47916666475470038, -3.267949192431252037 ) ) ;
#9028 = ORIENTED_EDGE ( 'NONE', *, *, #7486, .F. ) ;
#9029 = CARTESIAN_POINT ( 'NONE',  ( 2.472591809326055046, 28.89829686842209355, 15.51343341526694353 ) ) ;
#9030 = DIRECTION ( 'NONE',  ( -0.000000000000000000, -0.000000000000000000, 1.000000000000000000 ) ) ;
#9031 = LINE ( 'NONE', #7302, #1496 ) ;
#9032 = CARTESIAN_POINT ( 'NONE',  ( 4.000000000000003553, 4.286263797015736595E-16, -3.500000000000000000 ) ) ;
#9033 = DIRECTION ( 'NONE',  ( 1.000000000000000000, -0.000000000000000000, -0.000000000000000000 ) ) ;
#9034 = CARTESIAN_POINT ( 'NONE',  ( -25.98076211353311393, 55.31874999904394485, -3.128098921329806714 ) ) ;
#9035 = DIRECTION ( 'NONE',  ( 0.000000000000000000, 0.000000000000000000, -1.000000000000000000 ) ) ;
#9036 = DIRECTION ( 'NONE',  ( 0.000000000000000000, 0.000000000000000000, -1.000000000000000000 ) ) ;
#9037 = EDGE_LOOP ( 'NONE', ( #3566, #8021, #8892, #2697 ) ) ;
#9038 = CARTESIAN_POINT ( 'NONE',  ( 1.449747468305832898, 33.50000000000000000, 14.82812500000000355 ) ) ;
#9039 = DIRECTION ( 'NONE',  ( 0.000000000000000000, 0.000000000000000000, 1.000000000000000000 ) ) ;
#9040 = CARTESIAN_POINT ( 'NONE',  ( -24.35964822603314417, 50.59374999904394343, -5.000000000000103029 ) ) ;
#9041 = CARTESIAN_POINT ( 'NONE',  ( -27.60187600103308725, 55.02708333237728056, -4.064049460664955760 ) ) ;
#9042 = CARTESIAN_POINT ( 'NONE',  ( 20.73695268571362504, 18.16262921024512167, 12.00579112326941988 ) ) ;
#9043 = CARTESIAN_POINT ( 'NONE',  ( -24.35964822603314772, 55.37708333237728198, -5.935950539335252074 ) ) ;
#9044 = ORIENTED_EDGE ( 'NONE', *, *, #8871, .T. ) ;
#9045 = CARTESIAN_POINT ( 'NONE',  ( -27.60187600103308014, 55.78541666571062052, -5.935950539335252074 ) ) ;
#9046 = ORIENTED_EDGE ( 'NONE', *, *, #9598, .T. ) ;
#9047 = DIRECTION ( 'NONE',  ( -1.000000000000000000, 0.000000000000000000, 0.000000000000000000 ) ) ;
#9048 = EDGE_LOOP ( 'NONE', ( #8007, #8431, #8825, #5276 ) ) ;
#9049 = LINE ( 'NONE', #6590, #2384 ) ;
#9050 = ORIENTED_EDGE ( 'NONE', *, *, #2147, .T. ) ;
#9051 = CARTESIAN_POINT ( 'NONE',  ( 23.19605965318632457, 18.72439211931539660, 10.95195840513869179 ) ) ;
#9052 = EDGE_CURVE ( 'NONE', #4348, #58, #10374, .T. ) ;
#9053 = CARTESIAN_POINT ( 'NONE',  ( 4.236525694536557474, -2.416953475386482530, -3.751298745799839462 ) ) ;
#9054 = EDGE_CURVE ( 'NONE', #3173, #516, #5062, .T. ) ;
#9055 = CARTESIAN_POINT ( 'NONE',  ( 17.78598590678423719, 16.10215687441832699, 12.01726674494117653 ) ) ;
#9056 = CARTESIAN_POINT ( 'NONE',  ( -24.98076211353312814, 53.72916666475470038, -6.732050807568954909 ) ) ;
#9057 = CARTESIAN_POINT ( 'NONE',  ( 34.93719828579780540, 2.096102678619137905, -4.721690477507365813 ) ) ;
#9058 = CARTESIAN_POINT ( 'NONE',  ( 3.200000000000000178, 0.3418418480469731513, -3.499999999999999556 ) ) ;
#9059 = EDGE_LOOP ( 'NONE', ( #2051, #9205, #5827, #1719 ) ) ;
#9060 = CARTESIAN_POINT ( 'NONE',  ( -3.527408190673961386, 28.61642175733934224, 15.04468341526694175 ) ) ;
#9061 = ORIENTED_EDGE ( 'NONE', *, *, #6745, .T. ) ;
#9062 = CARTESIAN_POINT ( 'NONE',  ( 20.50876875457641546, 17.93645829877244680, 13.00425721518307576 ) ) ;
#9063 = EDGE_CURVE ( 'NONE', #9687, #10877, #7616, .T. ) ;
#9064 = AXIS2_PLACEMENT_3D ( 'NONE', #5152, #8533, #2186 ) ;
#9065 = DIRECTION ( 'NONE',  ( 3.865177154556031370E-17, 0.7071067811865462405, -0.7071067811865489050 ) ) ;
#9066 = CARTESIAN_POINT ( 'NONE',  ( -24.35964822603314417, 49.71874999904395054, -5.000000000000103029 ) ) ;
#9067 = CARTESIAN_POINT ( 'NONE',  ( -25.98076211353311393, 49.49999999999986500, -5.000000000000103029 ) ) ;
#9068 = CARTESIAN_POINT ( 'NONE',  ( -3.494791681227492397, 29.65833842083190675, 15.48578750830907147 ) ) ;
#9069 = CARTESIAN_POINT ( 'NONE',  ( -25.98076211353324894, 14.99999999999984190, -2.500000000000000000 ) ) ;
#9070 = CARTESIAN_POINT ( 'NONE',  ( 34.99999999999987210, 2.000000000000002220, -12.50000000000000000 ) ) ;
#9071 = DIRECTION ( 'NONE',  ( -0.000000000000000000, -0.000000000000000000, -1.000000000000000000 ) ) ;
#9072 = MANIFOLD_SOLID_BREP ( 'Hex', #4358 ) ;
#9073 = EDGE_LOOP ( 'NONE', ( #1602, #2795, #2491 ) ) ;
#9074 = CARTESIAN_POINT ( 'NONE',  ( -2.472591809326051937, 31.10170313157791000, 14.88843341526694353 ) ) ;
#9075 = DIRECTION ( 'NONE',  ( 0.000000000000000000, 0.000000000000000000, 1.000000000000000000 ) ) ;
#9076 = CARTESIAN_POINT ( 'NONE',  ( 21.21106610644839208, 53.49999999999983658, 2.500000000000000000 ) ) ;
#9077 = CARTESIAN_POINT ( 'NONE',  ( 3.200000000000000178, 0.000000000000000000, 0.000000000000000000 ) ) ;
#9078 = LINE ( 'NONE', #3366, #10137 ) ;
#9079 = CARTESIAN_POINT ( 'NONE',  ( -27.60187600103308014, 55.78541666571062052, -5.935950539335252074 ) ) ;
#9080 = ADVANCED_FACE ( 'NONE', ( #4899 ), #1923, .F. ) ;
#9081 = DIRECTION ( 'NONE',  ( -1.000000000000000000, -0.000000000000000000, -0.000000000000000000 ) ) ;
#9082 = DIRECTION ( 'NONE',  ( -0.000000000000000000, -0.000000000000000000, -1.000000000000000000 ) ) ;
#9083 = VERTEX_POINT ( 'NONE', #2137 ) ;
#9084 = CARTESIAN_POINT ( 'NONE',  ( -3.500000000000002665, 28.55025253169416288, 15.29687500000000533 ) ) ;
#9085 = VECTOR ( 'NONE', #5325, 1000.000000000000000 ) ;
#9086 = DIRECTION ( 'NONE',  ( 0.000000000000000000, -1.287488025362403787E-15, -1.000000000000000000 ) ) ;
#9087 = CARTESIAN_POINT ( 'NONE',  ( -27.60187600103308370, 50.94374999904394485, -5.000000000000103029 ) ) ;
#9088 = CARTESIAN_POINT ( 'NONE',  ( -25.17020516978313083, 54.03541666571061342, -6.403925809002825709 ) ) ;
#9089 = CARTESIAN_POINT ( 'NONE',  ( 17.59356678224322934, 17.35619608210146581, 12.08212522340233264 ) ) ;
#9090 = CARTESIAN_POINT ( 'NONE',  ( -24.98076211353312814, 50.31666666666652787, -6.732050807568954909 ) ) ;
#9091 = ORIENTED_EDGE ( 'NONE', *, *, #8603, .F. ) ;
#9092 = CARTESIAN_POINT ( 'NONE',  ( -24.35964822603314417, 55.49374999904394912, -5.000000000000103029 ) ) ;
#9093 = VERTEX_POINT ( 'NONE', #1555 ) ;
#9094 = ORIENTED_EDGE ( 'NONE', *, *, #10382, .T. ) ;
#9095 = DIRECTION ( 'NONE',  ( 0.6587175828649983744, -0.7523902883640206651, 4.024558464266192459E-16 ) ) ;
#9096 = ORIENTED_EDGE ( 'NONE', *, *, #9594, .F. ) ;
#9097 = DIRECTION ( 'NONE',  ( 2.775557561562891351E-17, 1.000000000000000000, -8.326672684688671588E-17 ) ) ;
#9098 = DIRECTION ( 'NONE',  ( 1.000000000000000000, 0.000000000000000000, 0.000000000000000000 ) ) ;
#9099 = ORIENTED_EDGE ( 'NONE', *, *, #2772, .T. ) ;
#9100 = CARTESIAN_POINT ( 'NONE',  ( 16.35082997044643704, 18.59891749786092063, 12.19867189564230969 ) ) ;
#9101 = EDGE_CURVE ( 'NONE', #1491, #7008, #3980, .T. ) ;
#9102 = CARTESIAN_POINT ( 'NONE',  ( 0.000000000000000000, 0.000000000000000000, 0.000000000000000000 ) ) ;
#9103 = DIRECTION ( 'NONE',  ( 0.000000000000000000, -1.000000000000000000, 9.783878858594328898E-16 ) ) ;
#9104 = CARTESIAN_POINT ( 'NONE',  ( 20.18549546789347460, 16.49528347911771675, 12.94888893485705061 ) ) ;
#9105 = CARTESIAN_POINT ( 'NONE',  ( -27.98076211353308551, 51.16249999808803750, -5.000000000000103029 ) ) ;
#9106 = CARTESIAN_POINT ( 'NONE',  ( 4.000000000000000000, -1.942223658245635809, -0.3516579909967643691 ) ) ;
#9107 = CARTESIAN_POINT ( 'NONE',  ( 2.981723757189264301, 1.693953258775802162, -3.499999999999999112 ) ) ;
#9108 = VERTEX_POINT ( 'NONE', #9996 ) ;
#9109 = CARTESIAN_POINT ( 'NONE',  ( 1.449747468305836673, 26.49999999999999289, 14.35937500000000711 ) ) ;
#9110 = VERTEX_POINT ( 'NONE', #6595 ) ;
#9111 = ADVANCED_FACE ( 'NONE', ( #2383 ), #4169, .T. ) ;
#9112 = CARTESIAN_POINT ( 'NONE',  ( 15.45532619834991017, 18.08020770756206019, 13.21853671947355302 ) ) ;
#9113 = AXIS2_PLACEMENT_3D ( 'NONE', #4720, #9086, #9141 ) ;
#9114 = EDGE_CURVE ( 'NONE', #7847, #3283, #5891, .T. ) ;
#9115 = DIRECTION ( 'NONE',  ( 1.000000000000000000, 6.098637220230964906E-17, 6.308085367188384325E-16 ) ) ;
#9116 = CARTESIAN_POINT ( 'NONE',  ( 34.76670834929980458, 4.038474554490624868, 2.651503408690715435 ) ) ;
#9117 = FACE_OUTER_BOUND ( 'NONE', #3936, .T. ) ;
#9118 = AXIS2_PLACEMENT_3D ( 'NONE', #8757, #5323, #7044 ) ;
#9119 = CARTESIAN_POINT ( 'NONE',  ( -3.500000000000001332, 29.93383077435482065, 15.47094158473306535 ) ) ;
#9120 = AXIS2_PLACEMENT_3D ( 'NONE', #7999, #10379, #7942 ) ;
#9121 = ORIENTED_EDGE ( 'NONE', *, *, #9415, .F. ) ;
#9122 = CARTESIAN_POINT ( 'NONE',  ( 4.000000000000000000, 2.309401076758497151, -5.000000000000000000 ) ) ;
#9123 = EDGE_CURVE ( 'NONE', #6966, #10149, #605, .T. ) ;
#9124 = ORIENTED_EDGE ( 'NONE', *, *, #9972, .F. ) ;
#9125 = CARTESIAN_POINT ( 'NONE',  ( 3.200000000000000178, 0.000000000000000000, 0.000000000000000000 ) ) ;
#9126 = CIRCLE ( 'NONE', #8241, 2.000000000000000888 ) ;
#9127 = DIRECTION ( 'NONE',  ( 0.000000000000000000, 0.000000000000000000, 1.000000000000000000 ) ) ;
#9128 = CARTESIAN_POINT ( 'NONE',  ( 17.79249663040192431, 17.21067465782413919, 12.06642298039558980 ) ) ;
#9129 = AXIS2_PLACEMENT_3D ( 'NONE', #5155, #5316, #8701 ) ;
#9130 = LINE ( 'NONE', #631, #7920 ) ;
#9131 = EDGE_CURVE ( 'NONE', #10149, #10824, #10202, .T. ) ;
#9132 = ADVANCED_FACE ( 'NONE', ( #9217 ), #1610, .T. ) ;
#9133 = CARTESIAN_POINT ( 'NONE',  ( -994.2085799786045754, 0.000000000000000000, 0.000000000000000000 ) ) ;
#9134 = CARTESIAN_POINT ( 'NONE',  ( -27.60187600103308014, 50.71041666571061768, -5.935950539335252074 ) ) ;
#9135 = CARTESIAN_POINT ( 'NONE',  ( -25.98076211353311393, 49.49999999999986500, -5.000000000000103029 ) ) ;
#9136 = CARTESIAN_POINT ( 'NONE',  ( 4.211405965630455661, 2.460463115436283932, -3.751298928144577882 ) ) ;
#9137 = CIRCLE ( 'NONE', #3827, 2.000000000000000888 ) ;
#9138 = EDGE_LOOP ( 'NONE', ( #43, #5100, #8434, #1014, #10670 ) ) ;
#9139 = CARTESIAN_POINT ( 'NONE',  ( -2.474873734152916338, 27.52512626584707789, 15.37500000000000355 ) ) ;
#9140 = AXIS2_PLACEMENT_3D ( 'NONE', #10862, #637, #10982 ) ;
#9141 = DIRECTION ( 'NONE',  ( 0.000000000000000000, 1.000000000000000000, -1.287488025362403787E-15 ) ) ;
#9142 = CARTESIAN_POINT ( 'NONE',  ( -25.98076211353310683, 51.11874999904394201, -3.128098921329806714 ) ) ;
#9143 = CARTESIAN_POINT ( 'NONE',  ( -25.17020516978313083, 53.33541666571061768, -6.403925809002825709 ) ) ;
#9144 = AXIS2_PLACEMENT_3D ( 'NONE', #1263, #2937, #9868 ) ;
#9145 = CARTESIAN_POINT ( 'NONE',  ( 17.13192716875488131, 17.81782029955189728, 12.12541829646253078 ) ) ;
#9146 = CARTESIAN_POINT ( 'NONE',  ( -26.98076211353309972, 52.53333333333319644, -6.732050807568954909 ) ) ;
#9147 = ORIENTED_EDGE ( 'NONE', *, *, #3231, .F. ) ;
#9148 = SURFACE_STYLE_FILL_AREA ( #6140 ) ;
#9149 = EDGE_CURVE ( 'NONE', #7883, #5054, #4160, .T. ) ;
#9150 = ADVANCED_FACE ( 'NONE', ( #6550 ), #7183, .T. ) ;
#9151 = VERTEX_POINT ( 'NONE', #5886 ) ;
#9152 = ORIENTED_EDGE ( 'NONE', *, *, #3434, .T. ) ;
#9153 = CARTESIAN_POINT ( 'NONE',  ( -4.211140560182196957, -2.431303136016552013, -3.745885042887436178 ) ) ;
#9154 = ORIENTED_EDGE ( 'NONE', *, *, #7859, .F. ) ;
#9155 = DIRECTION ( 'NONE',  ( -1.000000000000000000, 0.000000000000000000, 0.000000000000000000 ) ) ;
#9156 = DIRECTION ( 'NONE',  ( 1.000000000000000000, 0.000000000000000000, 0.000000000000000000 ) ) ;
#9157 = ORIENTED_EDGE ( 'NONE', *, *, #5551, .T. ) ;
#9158 = VECTOR ( 'NONE', #4586, 1000.000000000000000 ) ;
#9159 = CARTESIAN_POINT ( 'NONE',  ( 19.32262643072814967, 17.24627075153934541, 11.00732576902737492 ) ) ;
#9160 = CARTESIAN_POINT ( 'NONE',  ( 2.887392608830354757, -4.041451884327390331, 2.328390191177121598E-14 ) ) ;
#9161 = CARTESIAN_POINT ( 'NONE',  ( 23.38258886820915095, 18.73219245557438484, 12.94889058896590583 ) ) ;
#9162 = CARTESIAN_POINT ( 'NONE',  ( -27.98076211353308551, 53.20416666475470180, -6.154700538379338504 ) ) ;
#9163 = CARTESIAN_POINT ( 'NONE',  ( -26.51666049839534622, 53.49373926088289721, -3.000000000000131006 ) ) ;
#9164 = CARTESIAN_POINT ( 'NONE',  ( 2.887392608830370744, 2.020725942163657862, -3.499999999999999556 ) ) ;
#9165 = PRODUCT ( 'BR-590', 'BR-590', '', ( #2841 ) ) ;
#9166 = ORIENTED_EDGE ( 'NONE', *, *, #1354, .T. ) ;
#9167 = AXIS2_PLACEMENT_3D ( 'NONE', #5086, #901, #956 ) ;
#9168 = CARTESIAN_POINT ( 'NONE',  ( 17.31910053175343478, 17.63064693655086757, 11.10566822806672427 ) ) ;
#9169 = CARTESIAN_POINT ( 'NONE',  ( 2.521662442312485819, 32.42808502599335441, 15.74780841526694175 ) ) ;
#9170 = VERTEX_POINT ( 'NONE', #7238 ) ;
#9171 = CARTESIAN_POINT ( 'NONE',  ( 19.93275388331568365, 16.31952634560019888, 12.94889180291853492 ) ) ;
#9172 = DIRECTION ( 'NONE',  ( 0.000000000000000000, 0.000000000000000000, 1.000000000000000000 ) ) ;
#9173 = AXIS2_PLACEMENT_3D ( 'NONE', #5355, #8738, #1122 ) ;
#9174 = LINE ( 'NONE', #1570, #5352 ) ;
#9175 = DIRECTION ( 'NONE',  ( 0.000000000000000000, 0.000000000000000000, 1.000000000000000000 ) ) ;
#9176 = B_SPLINE_CURVE_WITH_KNOTS ( 'NONE', 3,
 ( #3720, #4666, #7107, #3004 ),
 .UNSPECIFIED., .F., .F.,
 ( 4, 4 ),
 ( 0.000000000000000000, 1.000000000000000000 ),
 .UNSPECIFIED. ) ;
#9177 = CARTESIAN_POINT ( 'NONE',  ( -0.06616922564517727090, 32.50000000000000711, 12.65844158473306535 ) ) ;
#9178 = FACE_OUTER_BOUND ( 'NONE', #4465, .T. ) ;
#9179 = FACE_BOUND ( 'NONE', #5146, .T. ) ;
#9180 = CARTESIAN_POINT ( 'NONE',  ( 0.000000000000000000, 0.000000000000000000, 0.000000000000000000 ) ) ;
#9181 = ORIENTED_EDGE ( 'NONE', *, *, #9464, .F. ) ;
#9182 = EDGE_CURVE ( 'NONE', #7578, #4891, #3279, .T. ) ;
#9183 = ORIENTED_EDGE ( 'NONE', *, *, #5876, .T. ) ;
#9184 = COLOUR_RGB ( '', 0.40784314, 0.44705882, 0.49803922) ;
#9185 = MECHANICAL_DESIGN_GEOMETRIC_PRESENTATION_REPRESENTATION (  '', ( #9360 ), #9020 ) ;
#9186 = CARTESIAN_POINT ( 'NONE',  ( 0.2174200650117649736, 3.876582599186232603, 0.2855619784720455634 ) ) ;
#9187 = CARTESIAN_POINT ( 'NONE',  ( 4.000000000000000000, 2.309401076758497151, -3.433295621305379353 ) ) ;
#9188 = DIRECTION ( 'NONE',  ( -0.000000000000000000, -0.000000000000000000, -1.000000000000000000 ) ) ;
#9189 = EDGE_CURVE ( 'NONE', #1386, #7504, #10777, .T. ) ;
#9190 = PLANE ( 'NONE',  #10316 ) ;
#9191 = CARTESIAN_POINT ( 'NONE',  ( -26.79131905728310059, 54.56041666571061199, -3.596074190997381237 ) ) ;
#9192 = EDGE_CURVE ( 'NONE', #4635, #6934, #2388, .T. ) ;
#9193 = CARTESIAN_POINT ( 'NONE',  ( 1.312671235360372224, 3.860931062424219462, -0.05923475698270440348 ) ) ;
#9194 = VECTOR ( 'NONE', #4321, 1000.000000000000000 ) ;
#9195 = CARTESIAN_POINT ( 'NONE',  ( 4.000000000000000000, -1.677850389431204459, -3.535268758346977513 ) ) ;
#9196 = B_SPLINE_CURVE_WITH_KNOTS ( 'NONE', 3,
 ( #9285, #9454, #1847, #4297, #6675, #5901, #6846, #5080, #2638, #10898 ),
 .UNSPECIFIED., .F., .F.,
 ( 4, 2, 2, 2, 4 ),
 ( 0.004768944099797328175, 0.005165600962498952294, 0.005562257825200575545, 0.005958914687902199664, 0.006355571550603823783 ),
 .UNSPECIFIED. ) ;
#9197 = ORIENTED_EDGE ( 'NONE', *, *, #4200, .F. ) ;
#9198 = VECTOR ( 'NONE', #9961, 1000.000000000000000 ) ;
#9199 = CARTESIAN_POINT ( 'NONE',  ( 4.553649124439118623E-15, 27.49999999999999289, 14.28125000000000355 ) ) ;
#9200 = CARTESIAN_POINT ( 'NONE',  ( 5.560781378645575757, 0.000000000000000000, -4.000000000000000000 ) ) ;
#9201 = CARTESIAN_POINT ( 'NONE',  ( -26.79131905728310059, 51.76041666571061484, -3.596074190997381237 ) ) ;
#9202 = CARTESIAN_POINT ( 'NONE',  ( -26.79131905728310059, 54.15208333237728056, -6.403925809002825709 ) ) ;
#9203 = CARTESIAN_POINT ( 'NONE',  ( 16.89796509758404852, 18.05178237072099989, 12.14735994959144350 ) ) ;
#9204 = CARTESIAN_POINT ( 'NONE',  ( -27.98076211353308551, 53.29166666666653640, -6.154700538379338504 ) ) ;
#9205 = ORIENTED_EDGE ( 'NONE', *, *, #10410, .T. ) ;
#9206 = CARTESIAN_POINT ( 'NONE',  ( -26.51666049839534622, 54.10623925897106545, -3.000000000000131006 ) ) ;
#9207 = ORIENTED_EDGE ( 'NONE', *, *, #8138, .F. ) ;
#9208 = VERTEX_POINT ( 'NONE', #1835 ) ;
#9209 = FACE_OUTER_BOUND ( 'NONE', #2735, .T. ) ;
#9210 = B_SPLINE_CURVE_WITH_KNOTS ( 'NONE', 3,
 ( #588, #7378, #3935, #3156, #9987, #428 ),
 .UNSPECIFIED., .F., .F.,
 ( 4, 2, 4 ),
 ( 0.002044882221487522803, 0.003063384235218269934, 0.004081886248949017498 ),
 .UNSPECIFIED. ) ;
#9211 = ORIENTED_EDGE ( 'NONE', *, *, #5709, .T. ) ;
#9212 = CARTESIAN_POINT ( 'NONE',  ( -2.500000000000005773, 29.99999999999999645, 16.46875000000000355 ) ) ;
#9213 =( NAMED_UNIT ( * ) SI_UNIT ( $, .STERADIAN. ) SOLID_ANGLE_UNIT ( ) );
#9214 = ORIENTED_EDGE ( 'NONE', *, *, #3560, .F. ) ;
#9215 = CARTESIAN_POINT ( 'NONE',  ( 17.40659673382103989, 17.54313596447427770, 11.09746175923963918 ) ) ;
#9216 = PRESENTATION_STYLE_ASSIGNMENT (( #5834 ) ) ;
#9217 = FACE_OUTER_BOUND ( 'NONE', #3000, .T. ) ;
#9218 = DIRECTION ( 'NONE',  ( -1.000000000000000000, -0.000000000000000000, -0.000000000000000000 ) ) ;
#9219 = CARTESIAN_POINT ( 'NONE',  ( 16.65878245872646701, 16.87675144720473952, 12.10347664333366247 ) ) ;
#9220 = EDGE_CURVE ( 'NONE', #7610, #9110, #3504, .T. ) ;
#9221 = CARTESIAN_POINT ( 'NONE',  ( -25.98076211353311393, 50.06874999904394485, -6.871901078670400231 ) ) ;
#9222 = CARTESIAN_POINT ( 'NONE',  ( -4.207491450040567571, 2.029819825146470524, -3.671670828759566074 ) ) ;
#9223 = EDGE_LOOP ( 'NONE', ( #872, #7828, #8837 ) ) ;
#9224 = CARTESIAN_POINT ( 'NONE',  ( 29.49999999999999289, 5.000000000000001776, -2.500000000000000000 ) ) ;
#9225 = ORIENTED_EDGE ( 'NONE', *, *, #6615, .F. ) ;
#9226 = CARTESIAN_POINT ( 'NONE',  ( -3.500000000000003109, 29.99999999999999645, 13.96875000000000355 ) ) ;
#9227 = VERTEX_POINT ( 'NONE', #46 ) ;
#9228 = CARTESIAN_POINT ( 'NONE',  ( 19.79543838746868190, 16.23930471839911149, 12.94973781945951785 ) ) ;
#9229 = CARTESIAN_POINT ( 'NONE',  ( 22.08651808663882932, 17.88512374315008557, 11.95042449705224819 ) ) ;
#9230 = DIRECTION ( 'NONE',  ( 1.000000000000000000, 0.000000000000000000, 0.000000000000000000 ) ) ;
#9231 = CARTESIAN_POINT ( 'NONE',  ( 2.982579934988233372, 2.185595227304907073, 3.214438021527930012 ) ) ;
#9232 = CARTESIAN_POINT ( 'NONE',  ( 1.035533905932743970, 27.49999999999999289, 14.35937500000000711 ) ) ;
#9233 = CARTESIAN_POINT ( 'NONE',  ( -25.44486372867087454, 51.65623925897107682, -7.000000000000073719 ) ) ;
#9234 = DIRECTION ( 'NONE',  ( 1.000000000000000000, 6.098637220230964906E-17, 6.308085367188384325E-16 ) ) ;
#9235 = DIRECTION ( 'NONE',  ( -1.000000000000000000, -0.000000000000000000, -0.000000000000000000 ) ) ;
#9236 = VERTEX_POINT ( 'NONE', #8670 ) ;
#9237 = ORIENTED_EDGE ( 'NONE', *, *, #3161, .T. ) ;
#9238 = CARTESIAN_POINT ( 'NONE',  ( 34.99999999999987210, -3.999999999999989786, -4.999999999999999112 ) ) ;
#9239 = AXIS2_PLACEMENT_3D ( 'NONE', #9526, #2757, #6800 ) ;
#9240 = DIRECTION ( 'NONE',  ( 0.000000000000000000, 0.000000000000000000, -1.000000000000000000 ) ) ;
#9241 = CARTESIAN_POINT ( 'NONE',  ( 34.94170751511534689, 2.019541143081656998, -5.105981766738330485 ) ) ;
#9242 = UNCERTAINTY_MEASURE_WITH_UNIT (LENGTH_MEASURE( 1.000000000000000082E-05 ), #2, 'distance_accuracy_value', 'NONE');
#9243 = CARTESIAN_POINT ( 'NONE',  ( -1.767766952966370209, 28.23223304703362402, 15.37500000000000355 ) ) ;
#9244 = CARTESIAN_POINT ( 'NONE',  ( 25.98076211353324183, 54.99999999999984368, 2.500000000000000000 ) ) ;
#9245 = CARTESIAN_POINT ( 'NONE',  ( -25.17020516978313083, 54.91041666571061342, -6.403925809002825709 ) ) ;
#9246 = CARTESIAN_POINT ( 'NONE',  ( 0.3126073911696448659, -4.041451884327390331, 2.328673539876467720E-14 ) ) ;
#9247 = CARTESIAN_POINT ( 'NONE',  ( 4.000000000000000888, 0.8228435280416209752, -3.430609588141487976 ) ) ;
#9248 = CIRCLE ( 'NONE', #7473, 3.249999999999998668 ) ;
#9249 = VERTEX_POINT ( 'NONE', #5997 ) ;
#9250 = AXIS2_PLACEMENT_3D ( 'NONE', #9277, #6777, #53 ) ;
#9251 = FACE_OUTER_BOUND ( 'NONE', #3229, .T. ) ;
#9252 = CARTESIAN_POINT ( 'NONE',  ( -26.98076211353309972, 53.14583333142136468, -6.732050807568954909 ) ) ;
#9253 = ADVANCED_FACE ( 'NONE', ( #9330 ), #10332, .T. ) ;
#9254 = CARTESIAN_POINT ( 'NONE',  ( -27.60187600103308725, 55.20208333237727771, -4.064049460664955760 ) ) ;
#9255 = CARTESIAN_POINT ( 'NONE',  ( -25.17020516978313083, 52.63541666571061484, -6.403925809002825709 ) ) ;
#9256 = ADVANCED_FACE ( 'NONE', ( #2675 ), #1953, .T. ) ;
#9257 = DIRECTION ( 'NONE',  ( -0.7071067811865405783, -0.7071067811865545671, 0.000000000000000000 ) ) ;
#9258 = CARTESIAN_POINT ( 'NONE',  ( -27.98076211353308551, 53.40833333333319644, -3.845299461620869330 ) ) ;
#9259 = AXIS2_PLACEMENT_3D ( 'NONE', #7061, #995, #4404 ) ;
#9260 = EDGE_LOOP ( 'NONE', ( #2635, #8959 ) ) ;
#9261 = EDGE_LOOP ( 'NONE', ( #10046, #10950, #1902, #6287, #10236, #957 ) ) ;
#9262 = ORIENTED_EDGE ( 'NONE', *, *, #3161, .F. ) ;
#9263 = PLANE ( 'NONE',  #4701 ) ;
#9264 = ORIENTED_EDGE ( 'NONE', *, *, #8364, .T. ) ;
#9265 = EDGE_CURVE ( 'NONE', #6185, #10149, #6050, .T. ) ;
#9266 = DIRECTION ( 'NONE',  ( 0.000000000000000000, -0.5000000000000011102, -0.8660254037844379305 ) ) ;
#9267 = CARTESIAN_POINT ( 'NONE',  ( -38.99999999999985789, -4.000000000000057732, 9.999999999999968026 ) ) ;
#9268 = VERTEX_POINT ( 'NONE', #7891 ) ;
#9269 = CARTESIAN_POINT ( 'NONE',  ( 21.22493709936120254, 18.56951933379358621, 11.00732503135576401 ) ) ;
#9270 = DIRECTION ( 'NONE',  ( 0.000000000000000000, -0.5000000000000011102, -0.8660254037844379305 ) ) ;
#9271 = CIRCLE ( 'NONE', #2536, 0.1199999999999998845 ) ;
#9272 = CARTESIAN_POINT ( 'NONE',  ( -24.35964822603314772, 49.95208333237727771, -5.935950539335252074 ) ) ;
#9273 = EDGE_CURVE ( 'NONE', #750, #7348, #786, .T. ) ;
#9274 = CARTESIAN_POINT ( 'NONE',  ( 18.81331750051067075, 21.67874213615617762, 12.94889058896551326 ) ) ;
#9275 = CARTESIAN_POINT ( 'NONE',  ( 3.999999999999999112, 1.941961291383486277, -0.3515519931180248192 ) ) ;
#9276 = CARTESIAN_POINT ( 'NONE',  ( -27.98076211353308551, 54.72083333142136041, -3.845299461620869330 ) ) ;
#9277 = CARTESIAN_POINT ( 'NONE',  ( 0.000000000000000000, 0.000000000000000000, 2.500000000000000000 ) ) ;
#9278 = ORIENTED_EDGE ( 'NONE', *, *, #2276, .T. ) ;
#9279 = CARTESIAN_POINT ( 'NONE',  ( -26.98076211353309972, 50.57916666475469469, -3.267949192431252037 ) ) ;
#9280 = VERTEX_POINT ( 'NONE', #1722 ) ;
#9281 = CARTESIAN_POINT ( 'NONE',  ( 0.06616922564517879746, 26.50000000000000000, 14.53344158473306535 ) ) ;
#9282 = ORIENTED_EDGE ( 'NONE', *, *, #2676, .F. ) ;
#9283 = CARTESIAN_POINT ( 'NONE',  ( 22.63773560303409127, 18.20111046790825782, 12.94889058896590583 ) ) ;
#9284 = EDGE_CURVE ( 'NONE', #6429, #4729, #5282, .T. ) ;
#9285 = CARTESIAN_POINT ( 'NONE',  ( -25.98076211353311393, 59.00000000000083134, -7.000000000000074607 ) ) ;
#9286 = DIRECTION ( 'NONE',  ( 1.000000000000000000, -5.319818659662208633E-14, 0.000000000000000000 ) ) ;
#9287 = CARTESIAN_POINT ( 'NONE',  ( -27.60187600103308370, 51.46874999904395054, -5.000000000000103029 ) ) ;
#9288 = CARTESIAN_POINT ( 'NONE',  ( -1.035533905932736420, 27.49999999999998934, 15.45312500000000178 ) ) ;
#9289 = PLANE ( 'NONE',  #804 ) ;
#9290 = CYLINDRICAL_SURFACE ( 'NONE', #6639, 3.500000000000000000 ) ;
#9291 = DIRECTION ( 'NONE',  ( 1.000000000000000000, -0.000000000000000000, 1.156482317317871478E-16 ) ) ;
#9292 = ORIENTED_EDGE ( 'NONE', *, *, #553, .T. ) ;
#9293 = EDGE_LOOP ( 'NONE', ( #6717, #5704, #1563, #7650 ) ) ;
#9294 = FACE_OUTER_BOUND ( 'NONE', #6327, .T. ) ;
#9295 = CARTESIAN_POINT ( 'NONE',  ( 0.1217565302851138787, 3.710888496608923948, -0.5725525826504940241 ) ) ;
#9296 = CARTESIAN_POINT ( 'NONE',  ( 22.98009469009668138, 21.94211999725310491, 12.00579112326941988 ) ) ;
#9297 = CARTESIAN_POINT ( 'NONE',  ( 1.035533905932743970, 27.49999999999999289, 14.35937500000000533 ) ) ;
#9298 = DIRECTION ( 'NONE',  ( 2.775557561562891351E-17, 1.000000000000000000, -8.326672684688671588E-17 ) ) ;
#9299 = CARTESIAN_POINT ( 'NONE',  ( -25.17020516978313083, 54.73541666571062336, -6.403925809002825709 ) ) ;
#9300 = AXIS2_PLACEMENT_3D ( 'NONE', #4892, #8165, #3059 ) ;
#9301 = CARTESIAN_POINT ( 'NONE',  ( 25.71106610644839208, 0.000000000000000000, 10.00000000000000178 ) ) ;
#9302 = FACE_OUTER_BOUND ( 'NONE', #1001, .T. ) ;
#9303 = CARTESIAN_POINT ( 'NONE',  ( 0.000000000000000000, 2.449293598294706414E-16, 2.000000000000000000 ) ) ;
#9304 = VERTEX_POINT ( 'NONE', #4398 ) ;
#9305 = CARTESIAN_POINT ( 'NONE',  ( -27.98076211353308551, 50.49166666666652503, -6.154700538379338504 ) ) ;
#9306 = EDGE_CURVE ( 'NONE', #10078, #6093, #8383, .T. ) ;
#9307 = DIRECTION ( 'NONE',  ( 0.000000000000000000, 0.000000000000000000, 1.000000000000000000 ) ) ;
#9308 = AXIS2_PLACEMENT_3D ( 'NONE', #5976, #7647, #3591 ) ;
#9309 = CARTESIAN_POINT ( 'NONE',  ( -26.79131905728310059, 53.62708333237727487, -6.403925809002825709 ) ) ;
#9310 = ADVANCED_BREP_SHAPE_REPRESENTATION ( '', ( #1910, #308 ), #2282 ) ;
#9311 = CARTESIAN_POINT ( 'NONE',  ( -4.000000000000000000, -1.942223658245633811, -0.3516579909967644246 ) ) ;
#9312 = VECTOR ( 'NONE', #3600, 1000.000000000000000 ) ;
#9313 = DIRECTION ( 'NONE',  ( 0.000000000000000000, 0.5000000000000123235, 0.8660254037844314912 ) ) ;
#9314 = CARTESIAN_POINT ( 'NONE',  ( -27.98076211353308551, 53.99166666666653214, -6.154700538379338504 ) ) ;
#9315 = AXIS2_PLACEMENT_3D ( 'NONE', #9410, #5970, #787 ) ;
#9316 = ORIENTED_EDGE ( 'NONE', *, *, #5861, .F. ) ;
#9317 = EDGE_CURVE ( 'NONE', #4272, #3988, #5941, .T. ) ;
#9318 = ORIENTED_EDGE ( 'NONE', *, *, #2550, .F. ) ;
#9319 = VERTEX_POINT ( 'NONE', #9386 ) ;
#9320 = CARTESIAN_POINT ( 'NONE',  ( -25.98076211353324894, 14.99999999999984190, 2.500000000000000000 ) ) ;
#9321 = ORIENTED_EDGE ( 'NONE', *, *, #5330, .T. ) ;
#9322 = EDGE_CURVE ( 'NONE', #1489, #1717, #3610, .T. ) ;
#9323 = LINE ( 'NONE', #9381, #5930 ) ;
#9324 = CARTESIAN_POINT ( 'NONE',  ( 0.000000000000000000, 0.000000000000000000, 0.000000000000000000 ) ) ;
#9325 = AXIS2_PLACEMENT_3D ( 'NONE', #1246, #8744, #4588 ) ;
#9326 = ORIENTED_EDGE ( 'NONE', *, *, #107, .F. ) ;
#9327 = CARTESIAN_POINT ( 'NONE',  ( 20.47715220320264962, 17.98190999816754498, 12.00579112326941988 ) ) ;
#9328 = DIRECTION ( 'NONE',  ( -1.248995262339998101E-16, 0.7071067811865486830, 0.7071067811865463515 ) ) ;
#9329 = VECTOR ( 'NONE', #5156, 1000.000000000000000 ) ;
#9330 = FACE_OUTER_BOUND ( 'NONE', #8778, .T. ) ;
#9331 = LINE ( 'NONE', #4959, #4937 ) ;
#9332 = CARTESIAN_POINT ( 'NONE',  ( 16.14406960823794179, 17.39146429769401081, 11.14955153432450530 ) ) ;
#9333 = ADVANCED_FACE ( 'NONE', ( #10385 ), #4715, .F. ) ;
#9334 = DIRECTION ( 'NONE',  ( 0.000000000000000000, 0.000000000000000000, 1.000000000000000000 ) ) ;
#9335 = EDGE_CURVE ( 'NONE', #2292, #8489, #6531, .T. ) ;
#9336 = CARTESIAN_POINT ( 'NONE',  ( -26.98076211353309972, 54.07916666475470180, -3.267949192431252037 ) ) ;
#9337 = AXIS2_PLACEMENT_3D ( 'NONE', #6364, #9752, #2143 ) ;
#9338 = CARTESIAN_POINT ( 'NONE',  ( 0.000000000000000000, 0.000000000000000000, 2.500000000000000000 ) ) ;
#9339 = ORIENTED_EDGE ( 'NONE', *, *, #3701, .F. ) ;
#9340 = PLANE ( 'NONE',  #1018 ) ;
#9341 = ORIENTED_EDGE ( 'NONE', *, *, #920, .F. ) ;
#9342 = CARTESIAN_POINT ( 'NONE',  ( -3.494791681227492397, 29.65833842083190675, 15.48578750830907147 ) ) ;
#9343 = ORIENTED_EDGE ( 'NONE', *, *, #3291, .T. ) ;
#9344 = CARTESIAN_POINT ( 'NONE',  ( 22.48167088160742821, 22.45759571798082987, 13.00425721518307753 ) ) ;
#9345 = SURFACE_STYLE_USAGE ( .BOTH. , #2572 ) ;
#9346 = DIRECTION ( 'NONE',  ( -1.000000000000000000, -0.000000000000000000, -0.000000000000000000 ) ) ;
#9347 = CARTESIAN_POINT ( 'NONE',  ( 19.69775075566884226, 17.43975236193677603, 12.00579112326941988 ) ) ;
#9348 = CARTESIAN_POINT ( 'NONE',  ( -27.60187600103308370, 52.16874999904395338, -5.000000000000103029 ) ) ;
#9349 = CARTESIAN_POINT ( 'NONE',  ( -1.035533905932742638, 32.50000000000000000, 16.23437500000000355 ) ) ;
#9350 = AXIS2_PLACEMENT_3D ( 'NONE', #3445, #2496, #8271 ) ;
#9351 = CARTESIAN_POINT ( 'NONE',  ( 0.000000000000000000, 2.020725942163738686, 3.499999999999999556 ) ) ;
#9352 = LINE ( 'NONE', #4249, #2392 ) ;
#9353 = CARTESIAN_POINT ( 'NONE',  ( -26.98076211353408027, 58.06623402467567274, -6.732050807568390027 ) ) ;
#9354 = ORIENTED_EDGE ( 'NONE', *, *, #3732, .F. ) ;
#9355 = EDGE_LOOP ( 'NONE', ( #7954, #1548, #1732, #1621 ) ) ;
#9356 = B_SPLINE_CURVE_WITH_KNOTS ( 'NONE', 3,
 ( #1244, #10525, #7921, #5413 ),
 .UNSPECIFIED., .F., .F.,
 ( 4, 4 ),
 ( 2.380739282170373118E-07, 0.002044882221487527140 ),
 .UNSPECIFIED. ) ;
#9357 = LINE ( 'NONE', #7520, #8629 ) ;
#9358 = CARTESIAN_POINT ( 'NONE',  ( -3.999999999999999112, 1.539600717838996324, -3.300726591567078039 ) ) ;
#9359 = AXIS2_PLACEMENT_3D ( 'NONE', #8524, #8574, #2645 ) ;
#9360 = STYLED_ITEM ( 'NONE', ( #224 ), #6795 ) ;
#9361 = CARTESIAN_POINT ( 'NONE',  ( 20.08745147943499987, 17.71083118005251933, 12.00579112326941988 ) ) ;
#9362 = CARTESIAN_POINT ( 'NONE',  ( 2.500000000000010214, 28.96446609406726580, 15.76562500000000178 ) ) ;
#9363 = CARTESIAN_POINT ( 'NONE',  ( 4.140404888673277384, 2.228338276487440428, -3.686887068327033390 ) ) ;
#9364 = CARTESIAN_POINT ( 'NONE',  ( -26.79131905728310059, 53.68541666571061910, -3.596074190997381237 ) ) ;
#9365 = FILL_AREA_STYLE ('',( #5975 ) ) ;
#9366 = FACE_OUTER_BOUND ( 'NONE', #2078, .T. ) ;
#9367 = FACE_OUTER_BOUND ( 'NONE', #8432, .T. ) ;
#9368 = EDGE_LOOP ( 'NONE', ( #366, #6127, #5875, #8480 ) ) ;
#9369 = CARTESIAN_POINT ( 'NONE',  ( 0.000000000000000000, -1.773042676681341856, 2.276824562219559311E-15 ) ) ;
#9370 = MECHANICAL_DESIGN_GEOMETRIC_PRESENTATION_REPRESENTATION (  '', ( #3164 ), #3525 ) ;
#9371 = CARTESIAN_POINT ( 'NONE',  ( 25.98076211353324183, 54.99999999999984368, 2.500000000000000000 ) ) ;
#9372 = CARTESIAN_POINT ( 'NONE',  ( -27.60187600103308370, 52.34374999904394343, -5.000000000000103029 ) ) ;
#9373 = LINE ( 'NONE', #1771, #9492 ) ;
#9374 = AXIS2_PLACEMENT_3D ( 'NONE', #5518, #8853, #7078 ) ;
#9375 = CIRCLE ( 'NONE', #6182, 2.500000000000000444 ) ;
#9376 = DIRECTION ( 'NONE',  ( -0.000000000000000000, -0.000000000000000000, -1.000000000000000000 ) ) ;
#9377 = CARTESIAN_POINT ( 'NONE',  ( -27.98076211353308551, 50.54999999999986926, -5.000000000000103029 ) ) ;
#9378 = ORIENTED_EDGE ( 'NONE', *, *, #3422, .F. ) ;
#9379 = ORIENTED_EDGE ( 'NONE', *, *, #10789, .F. ) ;
#9380 = CARTESIAN_POINT ( 'NONE',  ( 7.623296525288699970E-18, 0.3418418480469747056, -3.499999999999999112 ) ) ;
#9381 = CARTESIAN_POINT ( 'NONE',  ( 29.50000000000000711, 2.000000000000001776, 17.49999999999999645 ) ) ;
#9382 = APPLICATION_PROTOCOL_DEFINITION ( 'draft international standard', 'automotive_design', 1998, #4593 ) ;
#9383 = ORIENTED_EDGE ( 'NONE', *, *, #754, .F. ) ;
#9384 = PLANE ( 'NONE',  #2072 ) ;
#9385 = DIRECTION ( 'NONE',  ( 8.659560562355001884E-17, -0.7071067811865420216, 0.7071067811865531239 ) ) ;
#9386 = CARTESIAN_POINT ( 'NONE',  ( 29.50000000000000711, 5.000000000000001776, 2.500000000000000000 ) ) ;
#9387 = DIRECTION ( 'NONE',  ( 1.000000000000000000, 0.000000000000000000, 0.000000000000000000 ) ) ;
#9388 = CARTESIAN_POINT ( 'NONE',  ( 21.04731615659443733, 17.16224689484156585, 11.95042449705224819 ) ) ;
#9389 = DIRECTION ( 'NONE',  ( 0.000000000000000000, 0.000000000000000000, 1.000000000000000000 ) ) ;
#9390 = CARTESIAN_POINT ( 'NONE',  ( -25.98076211353311393, 50.76874999904394770, -6.871901078670400231 ) ) ;
#9391 = CARTESIAN_POINT ( 'NONE',  ( 0.000000000000000000, 0.000000000000000000, 4.000000000000000000 ) ) ;
#9392 = ORIENTED_EDGE ( 'NONE', *, *, #5502, .T. ) ;
#9393 = LINE ( 'NONE', #6779, #2998 ) ;
#9394 = EDGE_LOOP ( 'NONE', ( #10513, #8844, #7260, #10049 ) ) ;
#9395 = CARTESIAN_POINT ( 'NONE',  ( -3.500000000000001332, 29.93383077435482065, 12.97094158473306358 ) ) ;
#9396 = ORIENTED_EDGE ( 'NONE', *, *, #10641, .F. ) ;
#9397 = CARTESIAN_POINT ( 'NONE',  ( 20.75790788474667181, 23.61206934513595357, 12.94889058896590583 ) ) ;
#9398 = EDGE_CURVE ( 'NONE', #3990, #1617, #1524, .T. ) ;
#9399 = EDGE_CURVE ( 'NONE', #4773, #4811, #10403, .T. ) ;
#9400 = CARTESIAN_POINT ( 'NONE',  ( 17.39179625728592882, 16.28601130006924791, 12.04260150961189524 ) ) ;
#9401 = CARTESIAN_POINT ( 'NONE',  ( 20.00651627240589647, 19.97666299463432438, 12.00579112326824216 ) ) ;
#9402 = CARTESIAN_POINT ( 'NONE',  ( -25.17020516978313083, 50.30208333237728624, -3.596074190997380349 ) ) ;
#9403 = CARTESIAN_POINT ( 'NONE',  ( 2.500000000000006661, 30.06616922564517580, 14.84594158473306713 ) ) ;
#9404 = FACE_OUTER_BOUND ( 'NONE', #9016, .T. ) ;
#9405 = CARTESIAN_POINT ( 'NONE',  ( 34.64101615137754919, 5.000000000000002665, 2.500000000000000000 ) ) ;
#9406 = ORIENTED_EDGE ( 'NONE', *, *, #4225, .T. ) ;
#9407 = ORIENTED_EDGE ( 'NONE', *, *, #10554, .T. ) ;
#9408 = CARTESIAN_POINT ( 'NONE',  ( 21.55579831881754416, 20.86490736922957367, 14.50000000000000000 ) ) ;
#9409 = EDGE_CURVE ( 'NONE', #10935, #1662, #7109, .T. ) ;
#9410 = CARTESIAN_POINT ( 'NONE',  ( 2.500000000000000000, 2.357898499370433054, -1.951563910473907981E-15 ) ) ;
#9411 = CARTESIAN_POINT ( 'NONE',  ( 34.66939463810009414, 4.803388076618550606, -2.500000000000000888 ) ) ;
#9412 = CARTESIAN_POINT ( 'NONE',  ( -2.500000000000007550, 31.03553390593274131, 15.14062500000000355 ) ) ;
#9413 = DIRECTION ( 'NONE',  ( -0.000000000000000000, 0.000000000000000000, 1.000000000000000000 ) ) ;
#9414 = CARTESIAN_POINT ( 'NONE',  ( -25.98076211353311393, 52.34374999904395054, -3.128098921329806714 ) ) ;
#9415 = EDGE_CURVE ( 'NONE', #1215, #5059, #2044, .T. ) ;
#9416 = CARTESIAN_POINT ( 'NONE',  ( -25.98076211353324894, 16.50000000000026290, -5.000000000000000000 ) ) ;
#9417 = DIRECTION ( 'NONE',  ( -0.000000000000000000, -0.000000000000000000, -1.000000000000000000 ) ) ;
#9418 = DIRECTION ( 'NONE',  ( 1.000000000000000000, 6.098637220230963674E-17, 1.156482317317871478E-16 ) ) ;
#9419 = ORIENTED_EDGE ( 'NONE', *, *, #9806, .F. ) ;
#9420 = CARTESIAN_POINT ( 'NONE',  ( -27.98076211353308551, 54.02083333142136468, -3.845299461620869330 ) ) ;
#9421 = B_SPLINE_CURVE_WITH_KNOTS ( 'NONE', 3,
 ( #1464, #6677, #6610, #2346, #7572, #10733, #3128, #6734, #10012, #10962 ),
 .UNSPECIFIED., .F., .F.,
 ( 4, 2, 2, 2, 4 ),
 ( 0.004769787300783674168, 0.005166447011858126687, 0.005563106722932580073, 0.005959766434007033459, 0.006356426145081485977 ),
 .UNSPECIFIED. ) ;
#9422 = CARTESIAN_POINT ( 'NONE',  ( -26.51666049839535688, 50.40626073911683847, -7.000000000000074607 ) ) ;
#9423 = CARTESIAN_POINT ( 'NONE',  ( 29.49999999999999645, -3.999999999999983569, 8.350000000000019185 ) ) ;
#9424 = CARTESIAN_POINT ( 'NONE',  ( -25.98076211353310683, 53.56874999904394485, -6.871901078670399343 ) ) ;
#9425 = EDGE_CURVE ( 'NONE', #7800, #7683, #5415, .T. ) ;
#9426 = VECTOR ( 'NONE', #3481, 1000.000000000000000 ) ;
#9427 = AXIS2_PLACEMENT_3D ( 'NONE', #4288, #4170, #10286 ) ;
#9428 = CARTESIAN_POINT ( 'NONE',  ( 2.887392608830370744, 2.020725942163657862, -3.499999999999999556 ) ) ;
#9429 = CARTESIAN_POINT ( 'NONE',  ( -27.78268512908117671, 55.49961679590671793, -4.132201955500060642 ) ) ;
#9430 = ORIENTED_EDGE ( 'NONE', *, *, #4908, .T. ) ;
#9431 = VERTEX_POINT ( 'NONE', #8887 ) ;
#9432 = CARTESIAN_POINT ( 'NONE',  ( 25.58039891549807976, 2.000000000000001776, -12.50099999999999767 ) ) ;
#9433 = CYLINDRICAL_SURFACE ( 'NONE', #3977, 34.99999999999999289 ) ;
#9434 = APPLICATION_PROTOCOL_DEFINITION ( 'draft international standard', 'automotive_design', 1998, #9837 ) ;
#9435 = EDGE_LOOP ( 'NONE', ( #4974, #8212, #8527 ) ) ;
#9436 = CARTESIAN_POINT ( 'NONE',  ( 24.49999999999999289, -6.767949192431108152, -4.999999999999991118 ) ) ;
#9437 = CYLINDRICAL_SURFACE ( 'NONE', #1342, 2.149999999999990585 ) ;
#9438 = DIRECTION ( 'NONE',  ( 0.8660254037844398178, 0.000000000000000000, -0.4999999999999978351 ) ) ;
#9439 = VECTOR ( 'NONE', #5376, 1000.000000000000000 ) ;
#9440 = CARTESIAN_POINT ( 'NONE',  ( 19.12295744889739879, 19.47009535162641569, 11.95042449705107224 ) ) ;
#9441 = CARTESIAN_POINT ( 'NONE',  ( 29.50000000000000711, 16.00000000000000000, 1.499999999999902522 ) ) ;
#9442 = CARTESIAN_POINT ( 'NONE',  ( -26.98076211353309972, 53.84583333142136752, -6.732050807568954909 ) ) ;
#9443 = DIRECTION ( 'NONE',  ( -0.000000000000000000, -0.000000000000000000, -1.000000000000000000 ) ) ;
#9444 = ORIENTED_EDGE ( 'NONE', *, *, #4582, .T. ) ;
#9445 = DIRECTION ( 'NONE',  ( 0.000000000000000000, 0.000000000000000000, 1.000000000000000000 ) ) ;
#9446 = ADVANCED_FACE ( 'NONE', ( #9716 ), #374, .T. ) ;
#9447 = PRODUCT_DEFINITION_SHAPE ( 'NONE', 'NONE',  #10998 ) ;
#9448 = ORIENTED_EDGE ( 'NONE', *, *, #7918, .F. ) ;
#9449 = CARTESIAN_POINT ( 'NONE',  ( -3.500000000000003109, 29.99999999999999645, 15.21875000000000355 ) ) ;
#9450 = AXIS2_PLACEMENT_3D ( 'NONE', #5287, #477, #1378 ) ;
#9451 = EDGE_LOOP ( 'NONE', ( #3836, #9341 ) ) ;
#9452 = EDGE_CURVE ( 'NONE', #1598, #5575, #9601, .T. ) ;
#9453 = CARTESIAN_POINT ( 'NONE',  ( 19.38445574543743177, 22.63941596627307362, 11.95042449705263898 ) ) ;
#9454 = CARTESIAN_POINT ( 'NONE',  ( -25.84843596800915932, 59.00000000000083844, -7.000000000000073719 ) ) ;
#9455 = CARTESIAN_POINT ( 'NONE',  ( 20.73695268571362504, 18.16262921024512167, 12.00579112326941988 ) ) ;
#9456 = CARTESIAN_POINT ( 'NONE',  ( 25.49999999999999645, -3.999999999999983569, 10.00000000000000888 ) ) ;
#9457 = LINE ( 'NONE', #4300, #1568 ) ;
#9458 =( BOUNDED_CURVE ( )  B_SPLINE_CURVE ( 2, ( #6931, #8655, #1034, #4445, #7825, #200, #6986, #10371, #2605 ),
 .UNSPECIFIED., .F., .F. ) 
 B_SPLINE_CURVE_WITH_KNOTS ( ( 3, 2, 2, 2, 3 ),
 ( 0.8611111111111111605, 0.8703703703703703498, 0.8888888888888888395, 0.9074074074074074403, 0.9166666666666667407 ),
 .UNSPECIFIED. ) 
 CURVE ( )  GEOMETRIC_REPRESENTATION_ITEM ( )  RATIONAL_B_SPLINE_CURVE ( ( 0.9330127018922194093, 0.9330127018922197424, 1.000000000000000000, 0.8660254037844387076, 1.000000000000000000, 0.8660254037844387076, 1.000000000000000000, 0.9330127018922189652, 0.9330127018922194093 ) ) 
 REPRESENTATION_ITEM ( '' )  );
#9459 = FACE_OUTER_BOUND ( 'NONE', #7661, .T. ) ;
#9460 = EDGE_CURVE ( 'NONE', #2134, #6486, #5504, .T. ) ;
#9461 = ORIENTED_EDGE ( 'NONE', *, *, #98, .T. ) ;
#9462 = ORIENTED_EDGE ( 'NONE', *, *, #10489, .F. ) ;
#9463 =( REPRESENTATION_RELATIONSHIP ('NONE','NONE', #7540, #1223 ) REPRESENTATION_RELATIONSHIP_WITH_TRANSFORMATION ( #5605 )SHAPE_REPRESENTATION_RELATIONSHIP( ) );
#9464 = EDGE_CURVE ( 'NONE', #7695, #927, #9126, .T. ) ;
#9465 = CARTESIAN_POINT ( 'NONE',  ( 0.000000000000000000, -0.8865213383406694847, 1.535500000000001419 ) ) ;
#9466 = CYLINDRICAL_SURFACE ( 'NONE', #3821, 1.999999999999971356 ) ;
#9467 = CARTESIAN_POINT ( 'NONE',  ( 3.319999999999999840, 0.000000000000000000, -3.369999999999997886 ) ) ;
#9468 = CARTESIAN_POINT ( 'NONE',  ( -24.98076211353312814, 55.82916666475470180, -6.732050807568954909 ) ) ;
#9469 = CARTESIAN_POINT ( 'NONE',  ( 0.5449313310647804220, 4.304185902836899835, -3.316620875263383894 ) ) ;
#9470 = CARTESIAN_POINT ( 'NONE',  ( -25.98076211353311393, 53.39374999904394770, -6.871901078670400231 ) ) ;
#9471 = CARTESIAN_POINT ( 'NONE',  ( 29.49999999999999645, -7.999999999999996447, -12.49999999999999822 ) ) ;
#9472 = CARTESIAN_POINT ( 'NONE',  ( -24.98076211353223641, 57.86679757347771158, -3.267949192431767180 ) ) ;
#9473 = DIRECTION ( 'NONE',  ( -0.000000000000000000, -0.000000000000000000, -1.000000000000000000 ) ) ;
#9474 = EDGE_CURVE ( 'NONE', #2370, #6817, #5410, .T. ) ;
#9475 = VERTEX_POINT ( 'NONE', #1708 ) ;
#9476 = CARTESIAN_POINT ( 'NONE',  ( -2.500000000000007550, 30.06616922564517580, 16.21655841526694175 ) ) ;
#9477 = CARTESIAN_POINT ( 'NONE',  ( 4.197393957002303999, -0.4069871074557456780, -3.503767560748925813 ) ) ;
#9478 = EDGE_CURVE ( 'NONE', #7462, #9268, #9373, .T. ) ;
#9479 = EDGE_CURVE ( 'NONE', #234, #7800, #8422, .T. ) ;
#9480 = CARTESIAN_POINT ( 'NONE',  ( -24.35964822603314417, 54.09374999904395054, -5.000000000000103029 ) ) ;
#9481 = CARTESIAN_POINT ( 'NONE',  ( -27.60187600103308725, 55.61041666571062336, -5.935950539335252074 ) ) ;
#9482 = DIRECTION ( 'NONE',  ( -1.000000000000000000, 0.000000000000000000, 0.000000000000000000 ) ) ;
#9483 = CARTESIAN_POINT ( 'NONE',  ( -6.473970235329672780E-16, -4.862606272033106691, -3.745885042887442395 ) ) ;
#9484 = AXIS2_PLACEMENT_3D ( 'NONE', #10526, #7865, #1245 ) ;
#9485 = ORIENTED_EDGE ( 'NONE', *, *, #9957, .F. ) ;
#9486 = VERTEX_POINT ( 'NONE', #6810 ) ;
#9487 = FACE_BOUND ( 'NONE', #10591, .T. ) ;
#9488 = DIRECTION ( 'NONE',  ( 0.000000000000000000, -0.000000000000000000, -1.000000000000000000 ) ) ;
#9489 = SHAPE_DEFINITION_REPRESENTATION ( #5201, #716 ) ;
#9490 = ORIENTED_EDGE ( 'NONE', *, *, #1940, .F. ) ;
#9491 = FACE_OUTER_BOUND ( 'NONE', #7155, .T. ) ;
#9492 = VECTOR ( 'NONE', #922, 1000.000000000000227 ) ;
#9493 = CARTESIAN_POINT ( 'NONE',  ( -25.44486372867087809, 54.54373926088290858, -7.000000000000075495 ) ) ;
#9494 = VECTOR ( 'NONE', #8902, 1000.000000000000227 ) ;
#9495 = CIRCLE ( 'NONE', #10027, 2.149999999999988809 ) ;
#9496 = EDGE_CURVE ( 'NONE', #8683, #10232, #9947, .T. ) ;
#9497 = CARTESIAN_POINT ( 'NONE',  ( 19.48730207459018970, 19.05393922246432226, 11.95042449705224996 ) ) ;
#9498 = EDGE_CURVE ( 'NONE', #5409, #1804, #5269, .T. ) ;
#9499 = DIRECTION ( 'NONE',  ( 1.000000000000000000, -0.000000000000000000, -0.000000000000000000 ) ) ;
#9500 = CARTESIAN_POINT ( 'NONE',  ( -24.35964822603314772, 51.93541666571061199, -4.064049460664953983 ) ) ;
#9501 = AXIS2_PLACEMENT_3D ( 'NONE', #10858, #2308, #4024 ) ;
#9502 = DIRECTION ( 'NONE',  ( 0.000000000000000000, 0.000000000000000000, 1.000000000000000000 ) ) ;
#9503 = EDGE_LOOP ( 'NONE', ( #161, #1854 ) ) ;
#9504 = DIRECTION ( 'NONE',  ( -0.7071067811865479058, -0.7071067811865470176, 0.000000000000000000 ) ) ;
#9505 = ORIENTED_EDGE ( 'NONE', *, *, #8584, .F. ) ;
#9506 = CARTESIAN_POINT ( 'NONE',  ( -3.527408190673960053, 31.38357824266065066, 15.39281658473306358 ) ) ;
#9507 = CONICAL_SURFACE ( 'NONE', #2950, 3.499999999999999556, 1.047197551196603849 ) ;
#9508 = ORIENTED_EDGE ( 'NONE', *, *, #9877, .T. ) ;
#9509 = CARTESIAN_POINT ( 'NONE',  ( 23.22881793621964874, 18.67973499377871960, 11.95042449705234588 ) ) ;
#9510 = CARTESIAN_POINT ( 'NONE',  ( 29.49999999999999645, -3.999999999999986233, -6.649999999999986144 ) ) ;
#9511 = CARTESIAN_POINT ( 'NONE',  ( 23.17052989764754756, 21.62756661655841839, 12.00579112326981246 ) ) ;
#9513 = CARTESIAN_POINT ( 'NONE',  ( -25.98076211353311393, 51.29374999904394627, -6.871901078670400231 ) ) ;
#9512 = CIRCLE ( 'NONE', #10752, 2.149999999999992362 ) ;
#9514 = CARTESIAN_POINT ( 'NONE',  ( 2.500000000000000000, 1.768423874527822681, -1.021000000000002794 ) ) ;
#9515 = DIRECTION ( 'NONE',  ( 0.000000000000000000, 0.5000000000000011102, 0.8660254037844379305 ) ) ;
#9516 = DIRECTION ( 'NONE',  ( 0.000000000000000000, -1.000000000000000000, 0.000000000000000000 ) ) ;
#9517 = EDGE_LOOP ( 'NONE', ( #7678, #5233, #7490, #9326 ) ) ;
#9518 = ORIENTED_EDGE ( 'NONE', *, *, #6301, .F. ) ;
#9519 = DIRECTION ( 'NONE',  ( 1.000000000000000000, 0.000000000000000000, -0.000000000000000000 ) ) ;
#9521 = DIRECTION ( 'NONE',  ( -1.000000000000000000, -6.098637220230963674E-17, -1.156482317317871478E-16 ) ) ;
#9520 = CIRCLE ( 'NONE', #7213, 7.500000000000000000 ) ;
#9522 = CARTESIAN_POINT ( 'NONE',  ( -25.44486372867087454, 50.34373926088291284, -7.000000000000073719 ) ) ;
#9523 = PRODUCT_RELATED_PRODUCT_CATEGORY ( 'part', '', ( #9880 ) ) ;
#9524 = CARTESIAN_POINT ( 'NONE',  ( 2.500000000000000000, 0.000000000000000000, 2.041999999999999815 ) ) ;
#9525 =( BOUNDED_CURVE ( )  B_SPLINE_CURVE ( 2, ( #2219, #536, #5614, #8161, #9532, #9420, #5263, #9206, #6035 ),
 .UNSPECIFIED., .F., .T. ) 
 B_SPLINE_CURVE_WITH_KNOTS ( ( 3, 2, 2, 2, 3 ),
 ( 0.5833333333333333703, 0.5925925925925925597, 0.6111111111111111605, 0.6296296296296296502, 0.6388888888888889506 ),
 .UNSPECIFIED. ) 
 CURVE ( )  GEOMETRIC_REPRESENTATION_ITEM ( )  RATIONAL_B_SPLINE_CURVE ( ( 0.9330127018922194093, 0.9330127018922197424, 1.000000000000000000, 0.8660254037844387076, 1.000000000000000000, 0.8660254037844387076, 1.000000000000000000, 0.9330127018922189652, 0.9330127018922194093 ) ) 
 REPRESENTATION_ITEM ( '' )  );
#9526 = CARTESIAN_POINT ( 'NONE',  ( 29.49999999999999645, 5.000000000000001776, -5.500000000000000000 ) ) ;
#9527 = CARTESIAN_POINT ( 'NONE',  ( -27.60187600103308014, 52.11041666571061626, -5.935950539335252074 ) ) ;
#9528 = DIRECTION ( 'NONE',  ( -0.000000000000000000, -0.000000000000000000, -1.000000000000000000 ) ) ;
#9529 = CARTESIAN_POINT ( 'NONE',  ( 1.567478505476134606E-15, 4.618802153517012066, -3.433295621305382905 ) ) ;
#9530 = CARTESIAN_POINT ( 'NONE',  ( -21.65063509461104374, 12.49999999999986322, 2.500000000000000000 ) ) ;
#9531 = ORIENTED_EDGE ( 'NONE', *, *, #225, .F. ) ;
#9532 = CARTESIAN_POINT ( 'NONE',  ( -27.98076211353308551, 53.96249999808803466, -5.000000000000103029 ) ) ;
#9533 = CARTESIAN_POINT ( 'NONE',  ( -0.06616922564517033201, 27.49999999999998934, 16.52905841526693820 ) ) ;
#9534 = FACE_OUTER_BOUND ( 'NONE', #3413, .T. ) ;
#9535 = UNCERTAINTY_MEASURE_WITH_UNIT (LENGTH_MEASURE( 1.000000000000000082E-05 ), #5567, 'distance_accuracy_value', 'NONE');
#9536 = LINE ( 'NONE', #4494, #10721 ) ;
#9537 = EDGE_CURVE ( 'NONE', #5562, #7462, #10321, .T. ) ;
#9538 = CARTESIAN_POINT ( 'NONE',  ( -25.17020516978313083, 55.20208333237728482, -3.596074190997380349 ) ) ;
#9539 = EDGE_CURVE ( 'NONE', #9793, #38, #2541, .T. ) ;
#9540 = PRODUCT_DEFINITION_SHAPE ( 'NONE', 'NONE',  #11001 ) ;
#9541 = CARTESIAN_POINT ( 'NONE',  ( 2.500000000000000000, 0.000000000000000000, 0.000000000000000000 ) ) ;
#9542 = CIRCLE ( 'NONE', #8122, 3.249999999999998224 ) ;
#9543 = VECTOR ( 'NONE', #7926, 1000.000000000000000 ) ;
#9544 = FACE_OUTER_BOUND ( 'NONE', #10616, .T. ) ;
#9545 = ORIENTED_EDGE ( 'NONE', *, *, #3552, .F. ) ;
#9546 = ORIENTED_EDGE ( 'NONE', *, *, #5467, .T. ) ;
#9547 = CARTESIAN_POINT ( 'NONE',  ( -24.98076211353312814, 50.92916666475470322, -6.732050807568954909 ) ) ;
#9548 = FACE_OUTER_BOUND ( 'NONE', #10210, .T. ) ;
#9549 = APPLICATION_PROTOCOL_DEFINITION ( 'draft international standard', 'automotive_design', 1998, #8134 ) ;
#9550 = ORIENTED_EDGE ( 'NONE', *, *, #3563, .T. ) ;
#9551 = AXIS2_PLACEMENT_3D ( 'NONE', #1137, #5489, #8756 ) ;
#9552 = LINE ( 'NONE', #1325, #7189 ) ;
#9553 = CARTESIAN_POINT ( 'NONE',  ( -25.98076211353311393, 51.68749999808803608, -7.000000000000073719 ) ) ;
#9554 = AXIS2_PLACEMENT_3D ( 'NONE', #5207, #8414, #8585 ) ;
#9555 = CARTESIAN_POINT ( 'NONE',  ( 19.52039169078502212, 17.38380627596665562, 11.00732402621840578 ) ) ;
#9556 = CARTESIAN_POINT ( 'NONE',  ( 26.25045812061784289, 53.49999999999983658, 10.00000000000000178 ) ) ;
#9557 = CARTESIAN_POINT ( 'NONE',  ( -26.79131905728310059, 52.22708333237727629, -6.403925809002825709 ) ) ;
#9558 = LINE ( 'NONE', #3096, #5555 ) ;
#9559 = ORIENTED_EDGE ( 'NONE', *, *, #5785, .T. ) ;
#9560 = CARTESIAN_POINT ( 'NONE',  ( 21.55579831881754416, 20.86490736922957367, 2.500000000000000444 ) ) ;
#9561 = EDGE_LOOP ( 'NONE', ( #7081, #6274, #9207, #4450, #8429, #7940 ) ) ;
#9562 = CARTESIAN_POINT ( 'NONE',  ( 1.814555661125942132, 28.27902175519319883, 13.43969158473306713 ) ) ;
#9563 = ORIENTED_EDGE ( 'NONE', *, *, #8447, .T. ) ;
#9564 = CARTESIAN_POINT ( 'NONE',  ( 24.35722724902042202, 20.98982846826517346, 11.95042449705185739 ) ) ;
#9565 = DIRECTION ( 'NONE',  ( 1.000000000000000000, 0.000000000000000000, 0.000000000000000000 ) ) ;
#9566 = EDGE_CURVE ( 'NONE', #6542, #5182, #2664, .T. ) ;
#9567 = DIRECTION ( 'NONE',  ( 1.000000000000000000, -0.000000000000000000, 1.156482317317871478E-16 ) ) ;
#9568 = CARTESIAN_POINT ( 'NONE',  ( 18.10462311893278553, 17.05669763433401087, 12.04589798090090902 ) ) ;
#9569 = CARTESIAN_POINT ( 'NONE',  ( -25.98076211353311393, 54.79374999904395338, -6.871901078670400231 ) ) ;
#9570 =( NAMED_UNIT ( * ) SI_UNIT ( $, .STERADIAN. ) SOLID_ANGLE_UNIT ( ) );
#9571 = CARTESIAN_POINT ( 'NONE',  ( 2.000000000000000000, -0.8865213383406694847, 1.535500000000001419 ) ) ;
#9572 = CARTESIAN_POINT ( 'NONE',  ( -21.21106610644865498, 16.50000000000026290, -9.500000000000000000 ) ) ;
#9573 = ORIENTED_EDGE ( 'NONE', *, *, #1181, .F. ) ;
#9574 = CARTESIAN_POINT ( 'NONE',  ( 17.13192716875488131, 17.81782029955189728, 12.12541829646253078 ) ) ;
#9575 = DIRECTION ( 'NONE',  ( -0.000000000000000000, -0.000000000000000000, -1.000000000000000000 ) ) ;
#9576 =( BOUNDED_SURFACE ( )  B_SPLINE_SURFACE ( 3, 3, ( 
 ( #8796, #4479, #7863, #235, #7028, #9574, #1182, #5358, #1124, #7919, #3533, #5197, #8577, #960, #2698, #4365, #6916, #10305, #6075, #10634, #3026, #613, #10680, #5577, #8960, #554, #8129, #7338, #451, #508, #1353, #9848, #7286, #6446, #7396, #3953, #10579, #3853, #6349, #8906, #4637, #394, #9743, #3124, #2240, #5632, #4009, #5524, #3796, #8177, #8022, #6289, #1297, #10727 ),
 ( #1243, #2135, #9905, #6502, #2917, #4691, #8070, #7236, #4751, #5470, #3904, #6400, #3073, #9686, #9794, #9018, #2183, #8861, #1409, #4801, #2079, #7181, #2295, #4851, #5686, #9062, #1457, #8224, #2975, #6559, #7453, #2341, #8456, #10007, #2462, #4912, #10842, #6785, #1567, #3233, #10180, #8395, #8284, #9344, #7567, #2397, #9958, #4242, #773, #2571, #4179, #4120, #671, #1739 ),
 ( #2511, #9112, #5135, #10070, #1509, #5078, #1, #10895, #5845, #6606, #5021, #10956, #5956, #3349, #5786, #4968, #4070, #6731, #837, #9228, #9171, #5900, #10790, #8515, #7509, #3289, #6671, #893, #10124, #1623, #9283, #7628, #1676, #3402, #8340, #4295, #3176, #5733, #719, #223, #1169, #8732, #4352, #8626, #118, #2686, #9397, #5186, #5346, #6175, #59, #6907, #4416, #9614 ),
 ( #3463, #2012, #7071, #6844, #10400, #6012, #6226, #6955, #1795, #1964, #7904, #7801, #10344, #3518, #1908, #5296, #2855, #4468, #10292, #1845, #8566, #8684, #1113, #2739, #7741, #2798, #7684, #5398, #175, #3571, #6113, #8782, #7850, #9509, #1058, #4516, #3620, #283, #5239, #7011, #9564, #3677, #10461, #10237, #2636, #948, #6062, #1004, #9453, #10566, #6275, #2067, #2227, #3062 ),
 ( #1286, #6492, #5514, #4739, #6392, #497, #384, #4790, #3893, #7277, #5674, #7168, #5456, #9835, #9670, #7958, #2963, #9006, #3942, #8167, #2906, #8012, #544, #7328, #2286, #6335, #3787, #8897, #7224, #7118, #10622, #4681, #2173, #9051, #9730, #8116, #2128, #10514, #8057, #10671, #335, #4572, #3015, #9894, #5622, #437, #10717, #9783, #1399, #3730, #1231, #8847, #3115, #3840 ),
 ( #4628, #5566, #8946, #1339, #6438, #10057, #9945, #9168, #9215, #4058, #597, #5885, #2444, #8439, #5833, #5773, #2329, #7439, #6769, #1608, #9159, #4896, #818, #2498, #4223, #10112, #4839, #9269, #3389, #3995, #1663, #5060, #1553, #2553, #7613, #5005, #6719, #8381, #8273, #10167, #6593, #3165, #8215, #9994, #3269, #5938, #1446, #6653, #657, #7386, #10775, #6549, #5722, #8328 ),
 ( #10831, #3216, #9100, #1494, #2380, #4957, #706, #4108, #7494, #10880, #757, #4158, #7553, #10940, #3331, #7933, #3502, #8817, #8036, #310, #2991, #6888, #2933, #6310, #1781, #9327, #10220, #1720, #2037, #5225, #7200, #6250, #4335, #4280, #2617, #9643, #10595, #2877, #7986, #7724, #5430, #3447, #3705, #1259, #7143, #44, #10276, #5119, #7669, #2673, #10485, #7094, #4546, #10538 ) ),
 .UNSPECIFIED., .T., .F., .F. ) 
 B_SPLINE_SURFACE_WITH_KNOTS ( ( 4, 3, 4 ),
 ( 4, 2, 2, 2, 2, 2, 2, 2, 2, 2, 2, 2, 2, 2, 2, 2, 2, 2, 2, 2, 2, 2, 2, 2, 2, 2, 4 ),
 ( 0.000000000000000000, 0.5000000000000000000, 1.000000000000000000 ),
 ( 0.000000000000000000, 0.05059550242166081097, 0.08415034466705637040, 0.1009277657897541536, 0.1177051869124519229, 0.1353321994541143436, 0.1529592119957767782, 0.1882132370791016474, 0.2234672621624265165, 0.2410942747040889511, 0.2587212872457513857, 0.2827395206004625905, 0.3067577539551737398, 0.3547942206645960939, 0.4028306873740183924, 0.4268489207287295972, 0.4508671540834407465, 0.4680275555183331937, 0.4851879569532256964, 0.5195087598230107018, 0.5881503655625806015, 0.6567919713021505013, 0.7254335770417204010, 0.7940751827812903008, 0.8627167885208602005, 0.9313583942604301003, 1.000000000000000000 ),
 .UNSPECIFIED. ) 
 GEOMETRIC_REPRESENTATION_ITEM ( )  RATIONAL_B_SPLINE_SURFACE ( (
 ( 1.000000000000000000, 1.000000000000000000, 1.000000000000000000, 1.000000000000000000, 1.000000000000000000, 1.000000000000000000, 1.000000000000000000, 1.000000000000000000, 1.000000000000000000, 1.000000000000000000, 1.000000000000000000, 1.000000000000000000, 1.000000000000000000, 1.000000000000000000, 1.000000000000000000, 1.000000000000000000, 1.000000000000000000, 1.000000000000000000, 1.000000000000000000, 1.000000000000000000, 1.000000000000000000, 1.000000000000000000, 1.000000000000000000, 1.000000000000000000, 1.000000000000000000, 1.000000000000000000, 1.000000000000000000, 1.000000000000000000, 1.000000000000000000, 1.000000000000000000, 1.000000000000000000, 1.000000000000000000, 1.000000000000000000, 1.000000000000000000, 1.000000000000000000, 1.000000000000000000, 1.000000000000000000, 1.000000000000000000, 1.000000000000000000, 1.000000000000000000, 1.000000000000000000, 1.000000000000000000, 1.000000000000000000, 1.000000000000000000, 1.000000000000000000, 1.000000000000000000, 1.000000000000000000, 1.000000000000000000, 1.000000000000000000, 1.000000000000000000, 1.000000000000000000, 1.000000000000000000, 1.000000000000000000, 1.000000000000000000),
 ( 0.3333333333333333703, 0.3333333333333333703, 0.3333333333333333703, 0.3333333333333333703, 0.3333333333333333703, 0.3333333333333333703, 0.3333333333333333703, 0.3333333333333333703, 0.3333333333333333703, 0.3333333333333333703, 0.3333333333333333703, 0.3333333333333333703, 0.3333333333333333703, 0.3333333333333333703, 0.3333333333333333703, 0.3333333333333333703, 0.3333333333333333703, 0.3333333333333333703, 0.3333333333333333703, 0.3333333333333333703, 0.3333333333333333703, 0.3333333333333333703, 0.3333333333333333703, 0.3333333333333333703, 0.3333333333333333703, 0.3333333333333333703, 0.3333333333333333703, 0.3333333333333333703, 0.3333333333333333703, 0.3333333333333333703, 0.3333333333333333703, 0.3333333333333333703, 0.3333333333333333703, 0.3333333333333333703, 0.3333333333333333703, 0.3333333333333333703, 0.3333333333333333703, 0.3333333333333333703, 0.3333333333333333703, 0.3333333333333333703, 0.3333333333333333703, 0.3333333333333333703, 0.3333333333333333703, 0.3333333333333333703, 0.3333333333333333703, 0.3333333333333333703, 0.3333333333333333703, 0.3333333333333333703, 0.3333333333333333703, 0.3333333333333333703, 0.3333333333333333703, 0.3333333333333333703, 0.3333333333333333703, 0.3333333333333333703),
 ( 0.3333333333333333703, 0.3333333333333333703, 0.3333333333333333703, 0.3333333333333333703, 0.3333333333333333703, 0.3333333333333333703, 0.3333333333333333703, 0.3333333333333333703, 0.3333333333333333703, 0.3333333333333333703, 0.3333333333333333703, 0.3333333333333333703, 0.3333333333333333703, 0.3333333333333333703, 0.3333333333333333703, 0.3333333333333333703, 0.3333333333333333703, 0.3333333333333333703, 0.3333333333333333703, 0.3333333333333333703, 0.3333333333333333703, 0.3333333333333333703, 0.3333333333333333703, 0.3333333333333333703, 0.3333333333333333703, 0.3333333333333333703, 0.3333333333333333703, 0.3333333333333333703, 0.3333333333333333703, 0.3333333333333333703, 0.3333333333333333703, 0.3333333333333333703, 0.3333333333333333703, 0.3333333333333333703, 0.3333333333333333703, 0.3333333333333333703, 0.3333333333333333703, 0.3333333333333333703, 0.3333333333333333703, 0.3333333333333333703, 0.3333333333333333703, 0.3333333333333333703, 0.3333333333333333703, 0.3333333333333333703, 0.3333333333333333703, 0.3333333333333333703, 0.3333333333333333703, 0.3333333333333333703, 0.3333333333333333703, 0.3333333333333333703, 0.3333333333333333703, 0.3333333333333333703, 0.3333333333333333703, 0.3333333333333333703),
 ( 1.000000000000000000, 1.000000000000000000, 1.000000000000000000, 1.000000000000000000, 1.000000000000000000, 1.000000000000000000, 1.000000000000000000, 1.000000000000000000, 1.000000000000000000, 1.000000000000000000, 1.000000000000000000, 1.000000000000000000, 1.000000000000000000, 1.000000000000000000, 1.000000000000000000, 1.000000000000000000, 1.000000000000000000, 1.000000000000000000, 1.000000000000000000, 1.000000000000000000, 1.000000000000000000, 1.000000000000000000, 1.000000000000000000, 1.000000000000000000, 1.000000000000000000, 1.000000000000000000, 1.000000000000000000, 1.000000000000000000, 1.000000000000000000, 1.000000000000000000, 1.000000000000000000, 1.000000000000000000, 1.000000000000000000, 1.000000000000000000, 1.000000000000000000, 1.000000000000000000, 1.000000000000000000, 1.000000000000000000, 1.000000000000000000, 1.000000000000000000, 1.000000000000000000, 1.000000000000000000, 1.000000000000000000, 1.000000000000000000, 1.000000000000000000, 1.000000000000000000, 1.000000000000000000, 1.000000000000000000, 1.000000000000000000, 1.000000000000000000, 1.000000000000000000, 1.000000000000000000, 1.000000000000000000, 1.000000000000000000),
 ( 0.3333333333333333703, 0.3333333333333333703, 0.3333333333333333703, 0.3333333333333333703, 0.3333333333333333703, 0.3333333333333333703, 0.3333333333333333703, 0.3333333333333333703, 0.3333333333333333703, 0.3333333333333333703, 0.3333333333333333703, 0.3333333333333333703, 0.3333333333333333703, 0.3333333333333333703, 0.3333333333333333703, 0.3333333333333333703, 0.3333333333333333703, 0.3333333333333333703, 0.3333333333333333703, 0.3333333333333333703, 0.3333333333333333703, 0.3333333333333333703, 0.3333333333333333703, 0.3333333333333333703, 0.3333333333333333703, 0.3333333333333333703, 0.3333333333333333703, 0.3333333333333333703, 0.3333333333333333703, 0.3333333333333333703, 0.3333333333333333703, 0.3333333333333333703, 0.3333333333333333703, 0.3333333333333333703, 0.3333333333333333703, 0.3333333333333333703, 0.3333333333333333703, 0.3333333333333333703, 0.3333333333333333703, 0.3333333333333333703, 0.3333333333333333703, 0.3333333333333333703, 0.3333333333333333703, 0.3333333333333333703, 0.3333333333333333703, 0.3333333333333333703, 0.3333333333333333703, 0.3333333333333333703, 0.3333333333333333703, 0.3333333333333333703, 0.3333333333333333703, 0.3333333333333333703, 0.3333333333333333703, 0.3333333333333333703),
 ( 0.3333333333333333703, 0.3333333333333333703, 0.3333333333333333703, 0.3333333333333333703, 0.3333333333333333703, 0.3333333333333333703, 0.3333333333333333703, 0.3333333333333333703, 0.3333333333333333703, 0.3333333333333333703, 0.3333333333333333703, 0.3333333333333333703, 0.3333333333333333703, 0.3333333333333333703, 0.3333333333333333703, 0.3333333333333333703, 0.3333333333333333703, 0.3333333333333333703, 0.3333333333333333703, 0.3333333333333333703, 0.3333333333333333703, 0.3333333333333333703, 0.3333333333333333703, 0.3333333333333333703, 0.3333333333333333703, 0.3333333333333333703, 0.3333333333333333703, 0.3333333333333333703, 0.3333333333333333703, 0.3333333333333333703, 0.3333333333333333703, 0.3333333333333333703, 0.3333333333333333703, 0.3333333333333333703, 0.3333333333333333703, 0.3333333333333333703, 0.3333333333333333703, 0.3333333333333333703, 0.3333333333333333703, 0.3333333333333333703, 0.3333333333333333703, 0.3333333333333333703, 0.3333333333333333703, 0.3333333333333333703, 0.3333333333333333703, 0.3333333333333333703, 0.3333333333333333703, 0.3333333333333333703, 0.3333333333333333703, 0.3333333333333333703, 0.3333333333333333703, 0.3333333333333333703, 0.3333333333333333703, 0.3333333333333333703),
 ( 1.000000000000000000, 1.000000000000000000, 1.000000000000000000, 1.000000000000000000, 1.000000000000000000, 1.000000000000000000, 1.000000000000000000, 1.000000000000000000, 1.000000000000000000, 1.000000000000000000, 1.000000000000000000, 1.000000000000000000, 1.000000000000000000, 1.000000000000000000, 1.000000000000000000, 1.000000000000000000, 1.000000000000000000, 1.000000000000000000, 1.000000000000000000, 1.000000000000000000, 1.000000000000000000, 1.000000000000000000, 1.000000000000000000, 1.000000000000000000, 1.000000000000000000, 1.000000000000000000, 1.000000000000000000, 1.000000000000000000, 1.000000000000000000, 1.000000000000000000, 1.000000000000000000, 1.000000000000000000, 1.000000000000000000, 1.000000000000000000, 1.000000000000000000, 1.000000000000000000, 1.000000000000000000, 1.000000000000000000, 1.000000000000000000, 1.000000000000000000, 1.000000000000000000, 1.000000000000000000, 1.000000000000000000, 1.000000000000000000, 1.000000000000000000, 1.000000000000000000, 1.000000000000000000, 1.000000000000000000, 1.000000000000000000, 1.000000000000000000, 1.000000000000000000, 1.000000000000000000, 1.000000000000000000, 1.000000000000000000) ) ) 
 REPRESENTATION_ITEM ( '' )  SURFACE ( )  );
#9577 = FACE_OUTER_BOUND ( 'NONE', #5513, .T. ) ;
#9578 = CARTESIAN_POINT ( 'NONE',  ( -0.02511973781850462134, 4.877415612947412882, -3.751298745799839462 ) ) ;
#9579 = CARTESIAN_POINT ( 'NONE',  ( 6.098637220230963427E-16, -10.00000000000000000, -10.50000000000000355 ) ) ;
#9580 = CARTESIAN_POINT ( 'NONE',  ( 3.500000000000005773, 31.44974746830583356, 15.92187500000000178 ) ) ;
#9581 = DIRECTION ( 'NONE',  ( 1.000000000000000000, -0.000000000000000000, 1.156482317317871478E-16 ) ) ;
#9582 = ORIENTED_EDGE ( 'NONE', *, *, #4163, .F. ) ;
#9583 = DIRECTION ( 'NONE',  ( -1.000000000000000000, 0.000000000000000000, 0.000000000000000000 ) ) ;
#9584 = CARTESIAN_POINT ( 'NONE',  ( 2.500000000000007550, 31.03553390593274486, 14.67187500000000178 ) ) ;
#9585 = CARTESIAN_POINT ( 'NONE',  ( -26.98076211353309972, 53.37916666475469896, -3.267949192431252037 ) ) ;
#9586 = EDGE_CURVE ( 'NONE', #2547, #9083, #10206, .T. ) ;
#9587 = DIRECTION ( 'NONE',  ( -0.000000000000000000, 0.000000000000000000, 1.000000000000000000 ) ) ;
#9588 = CARTESIAN_POINT ( 'NONE',  ( -24.35964822603314772, 54.15208333237728766, -5.935950539335252074 ) ) ;
#9589 = LINE ( 'NONE', #1990, #10158 ) ;
#9590 = CARTESIAN_POINT ( 'NONE',  ( 3.200000000000000178, 0.000000000000000000, 0.000000000000000000 ) ) ;
#9591 = EDGE_LOOP ( 'NONE', ( #54, #1723 ) ) ;
#9592 = ORIENTED_EDGE ( 'NONE', *, *, #1940, .T. ) ;
#9593 = LINE ( 'NONE', #6095, #2200 ) ;
#9594 = EDGE_CURVE ( 'NONE', #3608, #8338, #9458, .T. ) ;
#9595 = CARTESIAN_POINT ( 'NONE',  ( 0.000000000000000000, 1.178949249685213863, -2.042000000000001148 ) ) ;
#9596 = DIRECTION ( 'NONE',  ( 0.000000000000000000, 0.000000000000000000, 1.000000000000000000 ) ) ;
#9597 = ORIENTED_EDGE ( 'NONE', *, *, #5467, .F. ) ;
#9598 = EDGE_CURVE ( 'NONE', #3312, #10201, #5947, .T. ) ;
#9599 = CARTESIAN_POINT ( 'NONE',  ( -25.98076211353311393, 49.49999999999986500, -7.000000000000074607 ) ) ;
#9600 = VECTOR ( 'NONE', #10793, 1000.000000000000000 ) ;
#9601 = LINE ( 'NONE', #5554, #9849 ) ;
#9602 = CARTESIAN_POINT ( 'NONE',  ( 23.08245441082096150, 20.10811672198468969, 11.00732503135576401 ) ) ;
#9603 = DIRECTION ( 'NONE',  ( -1.000000000000000000, -0.000000000000000000, -0.000000000000000000 ) ) ;
#9604 = CARTESIAN_POINT ( 'NONE',  ( -25.98076211353311393, 52.86874999904393491, -6.871901078670400231 ) ) ;
#9605 = ADVANCED_FACE ( 'NONE', ( #5982 ), #7599, .F. ) ;
#9606 = AXIS2_PLACEMENT_3D ( 'NONE', #6507, #2403, #4805 ) ;
#9607 = FACE_OUTER_BOUND ( 'NONE', #8560, .T. ) ;
#9608 = EDGE_LOOP ( 'NONE', ( #6667, #2376, #6587, #8164 ) ) ;
#9609 = CARTESIAN_POINT ( 'NONE',  ( 21.55579831881754416, 20.86490736922957367, 14.50000000000000000 ) ) ;
#9610 = ORIENTED_EDGE ( 'NONE', *, *, #4038, .T. ) ;
#9611 = CARTESIAN_POINT ( 'NONE',  ( 0.9693646802875628410, 32.52740819067395961, 13.83031658473306535 ) ) ;
#9612 = B_SPLINE_CURVE_WITH_KNOTS ( 'NONE', 3,
 ( #4981, #8355, #734, #1423 ),
 .UNSPECIFIED., .F., .F.,
 ( 4, 4 ),
 ( 0.000000000000000000, 0.002452478801916361129 ),
 .UNSPECIFIED. ) ;
#9613 = ORIENTED_EDGE ( 'NONE', *, *, #2558, .F. ) ;
#9614 = CARTESIAN_POINT ( 'NONE',  ( 19.44564476272491049, 19.01746825227115067, 12.94889058896590761 ) ) ;
#9615 = SHAPE_REPRESENTATION_RELATIONSHIP ( 'NONE' , 'NONE' ,  #75, #1232 ) ;
#9616 = EDGE_CURVE ( 'NONE', #6444, #7847, #6419, .T. ) ;
#9617 = EDGE_CURVE ( 'NONE', #9904, #6542, #7988, .T. ) ;
#9618 = CARTESIAN_POINT ( 'NONE',  ( 29.50000000000000711, -17.99999999999996803, 7.500000000000038192 ) ) ;
#9619 = CARTESIAN_POINT ( 'NONE',  ( 16.39761867860600475, 18.55212878970134938, 13.19648031090924789 ) ) ;
#9620 = CARTESIAN_POINT ( 'NONE',  ( -24.35964822603314417, 53.21874999904395764, -5.000000000000103029 ) ) ;
#9621 = CARTESIAN_POINT ( 'NONE',  ( -4.154094228333456762, 2.398367420968013253, -3.721909803043220055 ) ) ;
#9622 = AXIS2_PLACEMENT_3D ( 'NONE', #2421, #10653, #3043 ) ;
#9623 = DIRECTION ( 'NONE',  ( 0.000000000000000000, 0.000000000000000000, -1.000000000000000000 ) ) ;
#9624 = CARTESIAN_POINT ( 'NONE',  ( 24.49999999999999289, -3.999999999999986233, -7.767949192431114369 ) ) ;
#9625 = ORIENTED_EDGE ( 'NONE', *, *, #3404, .F. ) ;
#9626 = EDGE_CURVE ( 'NONE', #9782, #9720, #83, .T. ) ;
#9627 = DIRECTION ( 'NONE',  ( 1.000000000000000000, -2.212882687011047826E-16, 0.000000000000000000 ) ) ;
#9628 = FACE_OUTER_BOUND ( 'NONE', #1097, .T. ) ;
#9629 = PRODUCT_DEFINITION_SHAPE ( 'NONE', 'NONE',  #6528 ) ;
#9630 = DIRECTION ( 'NONE',  ( 0.000000000000000000, 0.000000000000000000, -1.000000000000000000 ) ) ;
#9631 = CARTESIAN_POINT ( 'NONE',  ( -23.98076211353314235, 49.49999999999986500, -5.000000000000103029 ) ) ;
#9632 = DIRECTION ( 'NONE',  ( 1.000000000000000000, 0.000000000000000000, 0.000000000000000000 ) ) ;
#9633 = CARTESIAN_POINT ( 'NONE',  ( -26.98076211353309972, 52.44583333142136894, -6.732050807568954909 ) ) ;
#9634 = DIRECTION ( 'NONE',  ( 1.000000000000000000, 8.881784197001252323E-16, 0.000000000000000000 ) ) ;
#9636 = ADVANCED_FACE ( 'NONE', ( #7201, #359 ), #5492, .T. ) ;
#9635 = LINE ( 'NONE', #2027, #668 ) ;
#9637 = CARTESIAN_POINT ( 'NONE',  ( 1.515916693951008254, 33.47259180932604750, 17.07593341526694530 ) ) ;
#9638 = CARTESIAN_POINT ( 'NONE',  ( -4.379688272585402942, 36.08837668307224789, 0.000000000000000000 ) ) ;
#9639 = ORIENTED_EDGE ( 'NONE', *, *, #793, .F. ) ;
#9640 = CARTESIAN_POINT ( 'NONE',  ( -1.767766952966375094, 31.76776695296636888, 15.06250000000000355 ) ) ;
#9641 =( BOUNDED_CURVE ( )  B_SPLINE_CURVE ( 2, ( #6837, #5892, #3341, #4234, #5179, #4345, #8559, #6901, #2084 ),
 .UNSPECIFIED., .F., .F. ) 
 B_SPLINE_CURVE_WITH_KNOTS ( ( 3, 2, 2, 2, 3 ),
 ( 0.6388888888888889506, 0.6481481481481481399, 0.6666666666666666297, 0.6851851851851852304, 0.6944444444444445308 ),
 .UNSPECIFIED. ) 
 CURVE ( )  GEOMETRIC_REPRESENTATION_ITEM ( )  RATIONAL_B_SPLINE_CURVE ( ( 0.9330127018922194093, 0.9330127018922197424, 1.000000000000000000, 0.8660254037844387076, 1.000000000000000000, 0.8660254037844387076, 1.000000000000000000, 0.9330127018922189652, 0.9330127018922194093 ) ) 
 REPRESENTATION_ITEM ( '' )  );
#9642 = CARTESIAN_POINT ( 'NONE',  ( 1.035533905932737975, 32.50000000000000711, 14.82812500000000178 ) ) ;
#9643 = CARTESIAN_POINT ( 'NONE',  ( 22.82387490247590733, 19.65457484615246386, 12.00579112326941988 ) ) ;
#9644 = FACE_OUTER_BOUND ( 'NONE', #1575, .T. ) ;
#9645 = CARTESIAN_POINT ( 'NONE',  ( -4.000000000000000000, 0.000000000000000000, 0.000000000000000000 ) ) ;
#9646 = FACE_OUTER_BOUND ( 'NONE', #9967, .T. ) ;
#9647 = CARTESIAN_POINT ( 'NONE',  ( -26.79131905728310059, 52.46041666571061768, -3.596074190997381237 ) ) ;
#9648 = CARTESIAN_POINT ( 'NONE',  ( 1.159276027961613812E-14, 2.686816014504609829, 2.346298152288358363 ) ) ;
#9649 = CARTESIAN_POINT ( 'NONE',  ( -27.98076211353308551, 54.80833333333318791, -3.845299461620869330 ) ) ;
#9650 = ORIENTED_EDGE ( 'NONE', *, *, #6361, .F. ) ;
#9651 = ADVANCED_FACE ( 'NONE', ( #4710 ), #1141, .F. ) ;
#9652 = ORIENTED_EDGE ( 'NONE', *, *, #2056, .T. ) ;
#9653 = FACE_OUTER_BOUND ( 'NONE', #7994, .T. ) ;
#9654 = ITEM_DEFINED_TRANSFORMATION ( 'NONE', 'NONE', #5102,  #308 ) ;
#9655 = EDGE_LOOP ( 'NONE', ( #3553, #5280, #2681 ) ) ;
#9656 = CIRCLE ( 'NONE', #246, 1.535500000000000087 ) ;
#9657 = FACE_OUTER_BOUND ( 'NONE', #552, .T. ) ;
#9658 = CARTESIAN_POINT ( 'NONE',  ( -26.79131905728310059, 50.65208333237728766, -6.403925809002825709 ) ) ;
#9659 = AXIS2_PLACEMENT_3D ( 'NONE', #9866, #6621, #5697 ) ;
#9660 = CARTESIAN_POINT ( 'NONE',  ( 22.42093126068789033, 23.47289781856171587, 10.95195840513859231 ) ) ;
#9661 = CIRCLE ( 'NONE', #9120, 1.650000000000000355 ) ;
#9662 = ORIENTED_EDGE ( 'NONE', *, *, #7841, .F. ) ;
#9663 = EDGE_CURVE ( 'NONE', #7719, #3723, #8092, .T. ) ;
#9664 = CARTESIAN_POINT ( 'NONE',  ( -26.79131905728310059, 54.56041666571061199, -3.596074190997381237 ) ) ;
#9665 = ORIENTED_EDGE ( 'NONE', *, *, #8829, .F. ) ;
#9666 = DIRECTION ( 'NONE',  ( -0.000000000000000000, 0.000000000000000000, -1.000000000000000000 ) ) ;
#9667 = ORIENTED_EDGE ( 'NONE', *, *, #1533, .F. ) ;
#9668 = CARTESIAN_POINT ( 'NONE',  ( 1.814555661125942132, 28.27902175519319883, 14.68969158473306535 ) ) ;
#9669 = ORIENTED_EDGE ( 'NONE', *, *, #1181, .T. ) ;
#9670 = CARTESIAN_POINT ( 'NONE',  ( 18.02930464311577907, 16.06944570838860642, 11.00389976449426399 ) ) ;
#9671 = FILL_AREA_STYLE_COLOUR ( '', #1029 ) ;
#9672 = VECTOR ( 'NONE', #9385, 999.9999999999998863 ) ;
#9673 = EDGE_CURVE ( 'NONE', #2508, #4738, #8745, .T. ) ;
#9674 = DIRECTION ( 'NONE',  ( 1.000000000000000000, -0.000000000000000000, -0.000000000000000000 ) ) ;
#9675 = EDGE_CURVE ( 'NONE', #7504, #7593, #10571, .T. ) ;
#9676 = B_SPLINE_CURVE_WITH_KNOTS ( 'NONE', 3,
 ( #2922, #6295, #9693, #2086, #9231, #10075 ),
 .UNSPECIFIED., .F., .F.,
 ( 4, 2, 4 ),
 ( 0.002044882221487527140, 0.003063384235218493713, 0.004081886248949459853 ),
 .UNSPECIFIED. ) ;
#9677 = CARTESIAN_POINT ( 'NONE',  ( 23.18216631463591781, 20.05868775325893338, 13.00425721518307753 ) ) ;
#9678 = CARTESIAN_POINT ( 'NONE',  ( -25.98076211353311393, 53.04374999904395338, -3.128098921329806714 ) ) ;
#9679 = AXIS2_PLACEMENT_3D ( 'NONE', #468, #4655, #8038 ) ;
#9680 = DIRECTION ( 'NONE',  ( 1.000000000000000000, 0.000000000000000000, 0.000000000000000000 ) ) ;
#9681 = VECTOR ( 'NONE', #3698, 1000.000000000000000 ) ;
#9682 = DIRECTION ( 'NONE',  ( 0.000000000000000000, 0.8660254037844380415, -0.5000000000000012212 ) ) ;
#9683 = CARTESIAN_POINT ( 'NONE',  ( -25.98076211353311393, 54.57499999999986073, -7.000000000000072831 ) ) ;
#9684 = ORIENTED_EDGE ( 'NONE', *, *, #3358, .F. ) ;
#9685 = ORIENTED_EDGE ( 'NONE', *, *, #5330, .F. ) ;
#9686 = CARTESIAN_POINT ( 'NONE',  ( 18.14679736200770677, 17.01284808935846371, 13.04404649446423115 ) ) ;
#9687 = VERTEX_POINT ( 'NONE', #9749 ) ;
#9688 = FACE_OUTER_BOUND ( 'NONE', #6482, .T. ) ;
#9689 = CARTESIAN_POINT ( 'NONE',  ( -23.98076211353314235, 50.19999999999986073, -5.000000000000103029 ) ) ;
#9690 = CIRCLE ( 'NONE', #10404, 2.499999999999999556 ) ;
#9691 = CARTESIAN_POINT ( 'NONE',  ( -25.98076211353415843, 59.00000000000900968, -2.999999999996041389 ) ) ;
#9692 = CARTESIAN_POINT ( 'NONE',  ( -6.259644161404860030E-16, -4.618802153517027165, -3.433295621305388234 ) ) ;
#9693 = CARTESIAN_POINT ( 'NONE',  ( 3.170065989602850909, 2.688325911136496771, 2.343682934607755008 ) ) ;
#9694 = CARTESIAN_POINT ( 'NONE',  ( 0.000000000000000000, 2.449293598294706414E-16, 2.000000000000000000 ) ) ;
#9695 = CARTESIAN_POINT ( 'NONE',  ( -2.474873734152920335, 32.47487373415291501, 15.06250000000000355 ) ) ;
#9696 = CARTESIAN_POINT ( 'NONE',  ( -25.98076211353310683, 54.92499999999986926, -3.000000000000132339 ) ) ;
#9697 = ORIENTED_EDGE ( 'NONE', *, *, #2080, .F. ) ;
#9698 = LINE ( 'NONE', #7091, #2980 ) ;
#9699 = AXIS2_PLACEMENT_3D ( 'NONE', #8497, #5995, #878 ) ;
#9700 = CARTESIAN_POINT ( 'NONE',  ( 3.500000000000007994, 29.93383077435482420, 16.84155841526694175 ) ) ;
#9701 = CARTESIAN_POINT ( 'NONE',  ( 2.500000000000007550, 31.03553390593274486, 15.92187500000000178 ) ) ;
#9702 = DIRECTION ( 'NONE',  ( 0.000000000000000000, 0.000000000000000000, 1.000000000000000000 ) ) ;
#9703 = DIRECTION ( 'NONE',  ( 1.000000000000000000, 0.000000000000000000, 0.000000000000000000 ) ) ;
#9704 = CARTESIAN_POINT ( 'NONE',  ( -4.000000000000000000, -1.560351142792950618, -0.2242961665059814425 ) ) ;
#9705 = CARTESIAN_POINT ( 'NONE',  ( 0.1750025118121568690, 4.719839900820621104, -3.469254087858248070 ) ) ;
#9706 = CARTESIAN_POINT ( 'NONE',  ( -25.98076211353311393, 51.46874999904394343, -6.871901078670400231 ) ) ;
#9707 = LINE ( 'NONE', #4713, #1639 ) ;
#9708 = DIRECTION ( 'NONE',  ( 0.000000000000000000, -0.8660254037844390407, -0.4999999999999994449 ) ) ;
#9709 = ORIENTED_EDGE ( 'NONE', *, *, #10498, .F. ) ;
#9710 = AXIS2_PLACEMENT_3D ( 'NONE', #9324, #10937, #6650 ) ;
#9711 = CARTESIAN_POINT ( 'NONE',  ( -27.98076211353308551, 54.74999999999985789, -5.000000000000103029 ) ) ;
#9712 = DIRECTION ( 'NONE',  ( 0.000000000000000000, 0.000000000000000000, 1.000000000000000000 ) ) ;
#9713 = APPLICATION_PROTOCOL_DEFINITION ( 'draft international standard', 'automotive_design', 1998, #4382 ) ;
#9714 = ORIENTED_EDGE ( 'NONE', *, *, #98, .F. ) ;
#9715 = CARTESIAN_POINT ( 'NONE',  ( 3.200000000000000178, 0.000000000000000000, 0.000000000000000000 ) ) ;
#9716 = FACE_OUTER_BOUND ( 'NONE', #3457, .T. ) ;
#9717 = CIRCLE ( 'NONE', #6161, 1.500000000000001332 ) ;
#9718 = AXIS2_PLACEMENT_3D ( 'NONE', #7278, #5623, #10718 ) ;
#9719 = CARTESIAN_POINT ( 'NONE',  ( 23.50695973324029353, 19.00259546466308791, 10.95195840513859231 ) ) ;
#9720 = VERTEX_POINT ( 'NONE', #411 ) ;
#9721 = CARTESIAN_POINT ( 'NONE',  ( -27.60187600103308014, 53.10208333237727629, -4.064049460664955760 ) ) ;
#9722 = ORIENTED_EDGE ( 'NONE', *, *, #524, .T. ) ;
#9723 = DIRECTION ( 'NONE',  ( 1.000000000000000000, -0.000000000000000000, -0.000000000000000000 ) ) ;
#9724 = ORIENTED_EDGE ( 'NONE', *, *, #4241, .T. ) ;
#9725 = VECTOR ( 'NONE', #1282, 1000.000000000000000 ) ;
#9726 = CARTESIAN_POINT ( 'NONE',  ( 2.500000000000010214, 28.96446609406726225, 14.51562500000000355 ) ) ;
#9727 =( NAMED_UNIT ( * ) SI_UNIT ( $, .STERADIAN. ) SOLID_ANGLE_UNIT ( ) );
#9728 = VERTEX_POINT ( 'NONE', #4549 ) ;
#9729 = AXIS2_PLACEMENT_3D ( 'NONE', #7870, #6136, #6298 ) ;
#9730 = CARTESIAN_POINT ( 'NONE',  ( 23.31046218964701211, 18.81639786330068276, 10.95195840513859231 ) ) ;
#9731 =( NAMED_UNIT ( * ) PLANE_ANGLE_UNIT ( ) SI_UNIT ( $, .RADIAN. ) );
#9732 = EDGE_CURVE ( 'NONE', #9017, #433, #4273, .T. ) ;
#9733 = DIRECTION ( 'NONE',  ( -4.312387734421997929E-17, 0.7071067811865487940, 0.7071067811865463515 ) ) ;
#9734 = AXIS2_PLACEMENT_3D ( 'NONE', #10709, #7430, #4885 ) ;
#9735 = CARTESIAN_POINT ( 'NONE',  ( 23.37401553338360571, 20.56828919810574519, 13.00425721518307753 ) ) ;
#9736 = VECTOR ( 'NONE', #616, 1000.000000000000000 ) ;
#9737 =( LENGTH_UNIT ( ) NAMED_UNIT ( * ) SI_UNIT ( .MILLI., .METRE. ) );
#9738 = CARTESIAN_POINT ( 'NONE',  ( 34.99999999999999289, -3.999999999999993339, 10.00000000000000533 ) ) ;
#9739 = CARTESIAN_POINT ( 'NONE',  ( -25.98076211353311393, 53.87499999999986500, -7.000000000000072831 ) ) ;
#9740 = VERTEX_POINT ( 'NONE', #4495 ) ;
#9741 = ORIENTED_EDGE ( 'NONE', *, *, #6832, .T. ) ;
#9742 = EDGE_CURVE ( 'NONE', #4891, #4976, #5540, .T. ) ;
#9743 = CARTESIAN_POINT ( 'NONE',  ( 22.98009469009668138, 21.94211999725310491, 12.00579112326941988 ) ) ;
#9744 = FACE_OUTER_BOUND ( 'NONE', #3784, .T. ) ;
#9745 = DIRECTION ( 'NONE',  ( 1.000000000000000000, 6.098637220230964906E-17, 0.000000000000000000 ) ) ;
#9746 = CARTESIAN_POINT ( 'NONE',  ( 29.50000000000000711, -9.999999999999998224, 15.49999999999998934 ) ) ;
#9747 = DIRECTION ( 'NONE',  ( -0.000000000000000000, -1.807003620809174139E-16, -1.000000000000000000 ) ) ;
#9748 = FACE_OUTER_BOUND ( 'NONE', #3952, .T. ) ;
#9749 = CARTESIAN_POINT ( 'NONE',  ( -25.98076211353311393, 50.02499999999987068, -3.000000000000132783 ) ) ;
#9750 = PRESENTATION_STYLE_ASSIGNMENT (( #3337 ) ) ;
#9751 = CARTESIAN_POINT ( 'NONE',  ( 3.500000000000007994, 28.55025253169416644, 14.51562500000000355 ) ) ;
#9752 = DIRECTION ( 'NONE',  ( -1.000000000000000000, -0.000000000000000000, -0.000000000000000000 ) ) ;
#9753 = ORIENTED_EDGE ( 'NONE', *, *, #4921, .F. ) ;
#9754 = FACE_BOUND ( 'NONE', #7552, .T. ) ;
#9755 = EDGE_CURVE ( 'NONE', #1715, #10456, #10650, .T. ) ;
#9756 = CARTESIAN_POINT ( 'NONE',  ( 1.515916693951008254, 33.47259180932604750, 15.82593341526694353 ) ) ;
#9757 = CARTESIAN_POINT ( 'NONE',  ( 1.814555661125939467, 31.72097824480680828, 16.99780841526693820 ) ) ;
#9758 = DIRECTION ( 'NONE',  ( 0.000000000000000000, 0.000000000000000000, -1.000000000000000000 ) ) ;
#9759 = CARTESIAN_POINT ( 'NONE',  ( 11.99999999999999645, 1.971681346627238735E-16, -1.610000000000000098 ) ) ;
#9760 = CARTESIAN_POINT ( 'NONE',  ( -23.98076211353314235, 53.55416666475470322, -3.845299461620867554 ) ) ;
#9761 = EDGE_CURVE ( 'NONE', #4515, #590, #1939, .T. ) ;
#9762 = DIRECTION ( 'NONE',  ( 0.000000000000000000, 1.000000000000000000, 0.000000000000000000 ) ) ;
#9763 = CARTESIAN_POINT ( 'NONE',  ( -24.35964822603314772, 51.93541666571061199, -4.064049460664953983 ) ) ;
#9764 = DIRECTION ( 'NONE',  ( 0.000000000000000000, 0.000000000000000000, 1.000000000000000000 ) ) ;
#9765 = CARTESIAN_POINT ( 'NONE',  ( 0.000000000000000000, 1.773042676681340524, -2.059984127722458425E-15 ) ) ;
#9766 = ORIENTED_EDGE ( 'NONE', *, *, #8797, .F. ) ;
#9767 = CARTESIAN_POINT ( 'NONE',  ( -1.144235203016679359, -3.958177651039096911, -0.09382832055446428676 ) ) ;
#9768 = CONTEXT_DEPENDENT_SHAPE_REPRESENTATION ( #7566, #831 ) ;
#9769 = ORIENTED_EDGE ( 'NONE', *, *, #1202, .F. ) ;
#9770 = EDGE_CURVE ( 'NONE', #8160, #10330, #853, .T. ) ;
#9771 = FACE_BOUND ( 'NONE', #1774, .T. ) ;
#9772 = CARTESIAN_POINT ( 'NONE',  ( 0.02993401039714445322, -3.373851915354637576, -1.156317065392215238 ) ) ;
#9773 = CARTESIAN_POINT ( 'NONE',  ( 18.06244887585786074, 17.10054717930957224, 11.04774946733758512 ) ) ;
#9774 = VERTEX_POINT ( 'NONE', #7468 ) ;
#9775 = DIRECTION ( 'NONE',  ( -1.000000000000000000, -0.000000000000000000, -0.000000000000000000 ) ) ;
#9776 = ORIENTED_EDGE ( 'NONE', *, *, #9761, .F. ) ;
#9777 = DIRECTION ( 'NONE',  ( -0.000000000000000000, 0.000000000000000000, 1.000000000000000000 ) ) ;
#9778 = ORIENTED_EDGE ( 'NONE', *, *, #10355, .T. ) ;
#9779 = CARTESIAN_POINT ( 'NONE',  ( 1.767766952966377314, 28.23223304703363112, 14.43750000000000178 ) ) ;
#9780 = PRESENTATION_STYLE_ASSIGNMENT (( #494 ) ) ;
#9781 = CIRCLE ( 'NONE', #6757, 2.500000000000000888 ) ;
#9782 = VERTEX_POINT ( 'NONE', #9032 ) ;
#9783 = CARTESIAN_POINT ( 'NONE',  ( 19.82941471729559524, 23.00258574805652856, 10.95195840513859231 ) ) ;
#9784 = CARTESIAN_POINT ( 'NONE',  ( 3.319999999999999840, 0.000000000000000000, 0.000000000000000000 ) ) ;
#9785 = CARTESIAN_POINT ( 'NONE',  ( 15.45532619834991017, 18.08020770756206019, 13.21853671947355302 ) ) ;
#9786 = AXIS2_PLACEMENT_3D ( 'NONE', #316, #8597, #10267 ) ;
#9787 = CARTESIAN_POINT ( 'NONE',  ( -27.98076211353308551, 52.50416666475469896, -6.154700538379338504 ) ) ;
#9788 = CARTESIAN_POINT ( 'NONE',  ( 24.49999999999999289, -3.999999999999986233, -4.999999999999992006 ) ) ;
#9789 = CARTESIAN_POINT ( 'NONE',  ( 34.99999999999999289, 7.372574772901430151E-15, 17.50000000000000355 ) ) ;
#9790 = EDGE_CURVE ( 'NONE', #7506, #10481, #7029, .T. ) ;
#9791 = PRODUCT_DEFINITION_SHAPE ( 'NONE', 'NONE',  #9799 ) ;
#9792 = ORIENTED_EDGE ( 'NONE', *, *, #7811, .T. ) ;
#9793 = VERTEX_POINT ( 'NONE', #6465 ) ;
#9794 = CARTESIAN_POINT ( 'NONE',  ( 18.31593954903570776, 16.96748919427588831, 13.03503021400358541 ) ) ;
#9795 = CARTESIAN_POINT ( 'NONE',  ( 29.49999999999999645, -3.999999999999986233, -4.999999999999991118 ) ) ;
#9796 = CARTESIAN_POINT ( 'NONE',  ( -27.98076211353308551, 49.84999999999986642, -5.000000000000103029 ) ) ;
#9797 = VECTOR ( 'NONE', #8305, 1000.000000000000000 ) ;
#9798 = LINE ( 'NONE', #4756, #547 ) ;
#9799 = PRODUCT_DEFINITION ( 'UNKNOWN', '', #6869, #7448 ) ;
#9800 = ADVANCED_FACE ( 'NONE', ( #3967 ), #684, .F. ) ;
#9801 = CARTESIAN_POINT ( 'NONE',  ( 4.000000000000000888, 1.563622288139206118, -0.2253451193528334950 ) ) ;
#9802 = CARTESIAN_POINT ( 'NONE',  ( 2.428085025993350410, 32.52166244231248271, 12.50219158473306358 ) ) ;
#9803 = DIRECTION ( 'NONE',  ( -1.000000000000000000, -6.098637220230963674E-17, 0.000000000000000000 ) ) ;
#9804 = VERTEX_POINT ( 'NONE', #2196 ) ;
#9805 = FACE_BOUND ( 'NONE', #4646, .T. ) ;
#9806 = EDGE_CURVE ( 'NONE', #4566, #1598, #4726, .T. ) ;
#9807 = CARTESIAN_POINT ( 'NONE',  ( -0.9693646802875689472, 32.52740819067395961, 15.98218341526694175 ) ) ;
#9808 = AXIS2_PLACEMENT_3D ( 'NONE', #3877, #10702, #3565 ) ;
#9809 = FACE_OUTER_BOUND ( 'NONE', #9059, .T. ) ;
#9810 = CARTESIAN_POINT ( 'NONE',  ( 16.58601566935801586, 18.36373179894819074, 12.17661548709639696 ) ) ;
#9811 = CARTESIAN_POINT ( 'NONE',  ( 34.99999999999999289, 16.00000000000000355, 1.499999999999947597 ) ) ;
#9812 = EDGE_CURVE ( 'NONE', #2901, #4949, #10029, .T. ) ;
#9813 = FACE_OUTER_BOUND ( 'NONE', #8905, .T. ) ;
#9814 = CARTESIAN_POINT ( 'NONE',  ( -27.60187600103308370, 53.74374999904394201, -5.000000000000103029 ) ) ;
#9815 = CARTESIAN_POINT ( 'NONE',  ( 0.6448876103708359731, 4.246476118072354922, -0.2256878752776725616 ) ) ;
#9816 = DIRECTION ( 'NONE',  ( -1.000000000000000000, -0.000000000000000000, -0.000000000000000000 ) ) ;
#9817 = ORIENTED_EDGE ( 'NONE', *, *, #8873, .F. ) ;
#9818 =( BOUNDED_CURVE ( )  B_SPLINE_CURVE ( 2, ( #3082, #6614, #2351, #782, #10850, #1468, #9027, #7349, #3241 ),
 .UNSPECIFIED., .F., .F. ) 
 B_SPLINE_CURVE_WITH_KNOTS ( ( 3, 2, 2, 2, 3 ),
 ( 0.8055555555555555802, 0.8148148148148147696, 0.8333333333333333703, 0.8518518518518518601, 0.8611111111111111605 ),
 .UNSPECIFIED. ) 
 CURVE ( )  GEOMETRIC_REPRESENTATION_ITEM ( )  RATIONAL_B_SPLINE_CURVE ( ( 0.9330127018922194093, 0.9330127018922197424, 1.000000000000000000, 0.8660254037844387076, 1.000000000000000000, 0.8660254037844387076, 1.000000000000000000, 0.9330127018922189652, 0.9330127018922194093 ) ) 
 REPRESENTATION_ITEM ( '' )  );
#9819 = CARTESIAN_POINT ( 'NONE',  ( -24.98076211353312814, 54.42916666475469611, -6.732050807568954909 ) ) ;
#9820 = CARTESIAN_POINT ( 'NONE',  ( -0.6448876103708541807, -4.246476118072358474, -0.2256878752776773356 ) ) ;
#9821 = ADVANCED_FACE ( 'NONE', ( #10805 ), #3919, .F. ) ;
#9822 = EDGE_CURVE ( 'NONE', #3429, #8693, #9130, .T. ) ;
#9823 = ORIENTED_EDGE ( 'NONE', *, *, #7851, .F. ) ;
#9824 = AXIS2_PLACEMENT_3D ( 'NONE', #1839, #2564, #5070 ) ;
#9825 = CARTESIAN_POINT ( 'NONE',  ( -24.35964822603314417, 51.29374999904394627, -5.000000000000103029 ) ) ;
#9826 = CARTESIAN_POINT ( 'NONE',  ( -27.60187600103308725, 50.01041666571062194, -5.935950539335252074 ) ) ;
#9827 = CARTESIAN_POINT ( 'NONE',  ( 23.31827848602400621, 20.57738196266585362, 12.00579112326941988 ) ) ;
#9828 = EDGE_LOOP ( 'NONE', ( #9903, #6906, #5718, #10375 ) ) ;
#9829 = CARTESIAN_POINT ( 'NONE',  ( 34.91780110604603493, 2.399866884679865198, 3.990594396599065341 ) ) ;
#9830 = ORIENTED_EDGE ( 'NONE', *, *, #9539, .F. ) ;
#9831 = CARTESIAN_POINT ( 'NONE',  ( 8.673617379884035472E-16, 4.618802153517012954, -5.000000000000000000 ) ) ;
#9832 = EDGE_LOOP ( 'NONE', ( #3973, #2892, #1146, #5893, #8324 ) ) ;
#9833 = LINE ( 'NONE', #9992, #600 ) ;
#9834 = EDGE_LOOP ( 'NONE', ( #5576, #2570, #3372, #6225, #9884, #6645, #9573, #9887, #2225, #10889 ) ) ;
#9835 = CARTESIAN_POINT ( 'NONE',  ( 17.74381166370891449, 16.14600641939347980, 11.01911823137775492 ) ) ;
#9836 =( NAMED_UNIT ( * ) SI_UNIT ( $, .STERADIAN. ) SOLID_ANGLE_UNIT ( ) );
#9837 = APPLICATION_CONTEXT ( 'automotive_design' ) ;
#9838 = EDGE_CURVE ( 'NONE', #2958, #6186, #2416, .T. ) ;
#9839 = VECTOR ( 'NONE', #1995, 1000.000000000000000 ) ;
#9840 = CYLINDRICAL_SURFACE ( 'NONE', #5463, 2.149999999999992362 ) ;
#9841 = CARTESIAN_POINT ( 'NONE',  ( 17.69587633286529282, 17.26453111358909354, 13.07531547515800874 ) ) ;
#9842 = CARTESIAN_POINT ( 'NONE',  ( -26.98076211353309972, 51.27916666475469754, -3.267949192431252037 ) ) ;
#9843 = AXIS2_PLACEMENT_3D ( 'NONE', #1126, #397, #3743 ) ;
#9844 = DIRECTION ( 'NONE',  ( 0.000000000000000000, 0.000000000000000000, -1.000000000000000000 ) ) ;
#9845 = CARTESIAN_POINT ( 'NONE',  ( 2.500000000000000000, -1.178949249685218303, -2.041999999999998039 ) ) ;
#9846 = ORIENTED_EDGE ( 'NONE', *, *, #6049, .F. ) ;
#9847 = ORIENTED_EDGE ( 'NONE', *, *, #4082, .T. ) ;
#9848 = CARTESIAN_POINT ( 'NONE',  ( 22.29575558078030895, 19.24694448270711788, 12.00579112326941988 ) ) ;
#9849 = VECTOR ( 'NONE', #4562, 999.9999999999998863 ) ;
#9850 = CARTESIAN_POINT ( 'NONE',  ( 29.49999999999999289, 16.00000000000000000, 1.499999999999945821 ) ) ;
#9851 = AXIS2_PLACEMENT_3D ( 'NONE', #5963, #5143, #7749 ) ;
#9852 = CARTESIAN_POINT ( 'NONE',  ( -26.51666049839534978, 49.70626073911682141, -7.000000000000073719 ) ) ;
#9854 = CARTESIAN_POINT ( 'NONE',  ( -25.18289562231869283, 57.38366758799607936, -6.836521581664483094 ) ) ;
#9853 = AXIS2_PLACEMENT_3D ( 'NONE', #10471, #4638, #2918 ) ;
#9855 = AXIS2_PLACEMENT_3D ( 'NONE', #4951, #9095, #4785 ) ;
#9856 = FACE_OUTER_BOUND ( 'NONE', #10006, .T. ) ;
#9857 = CARTESIAN_POINT ( 'NONE',  ( 2.521662442312487151, 27.57191497400665270, 13.43969158473306713 ) ) ;
#9858 = DIRECTION ( 'NONE',  ( 0.000000000000000000, 0.000000000000000000, 1.000000000000000000 ) ) ;
#9859 = UNCERTAINTY_MEASURE_WITH_UNIT (LENGTH_MEASURE( 1.000000000000000082E-05 ), #7500, 'distance_accuracy_value', 'NONE');
#9860 = EDGE_LOOP ( 'NONE', ( #1635, #506 ) ) ;
#9861 = CARTESIAN_POINT ( 'NONE',  ( 6.098637220230963427E-16, -10.00000000000000000, 0.000000000000000000 ) ) ;
#9862 = ORIENTED_EDGE ( 'NONE', *, *, #10957, .F. ) ;
#9863 = CARTESIAN_POINT ( 'NONE',  ( 1.101703131577913553, 32.47259180932605460, 15.82593341526694353 ) ) ;
#9864 = CIRCLE ( 'NONE', #1513, 4.999999999999997335 ) ;
#9865 = DIRECTION ( 'NONE',  ( 0.000000000000000000, 0.000000000000000000, 1.000000000000000000 ) ) ;
#9866 = CARTESIAN_POINT ( 'NONE',  ( 3.469446951953614189E-15, -1.040834085586084257E-14, 2.500000000000000000 ) ) ;
#9867 = DIRECTION ( 'NONE',  ( -1.000000000000000000, 0.000000000000000000, 0.000000000000000000 ) ) ;
#9868 = DIRECTION ( 'NONE',  ( -1.000000000000000000, 0.000000000000000000, -0.000000000000000000 ) ) ;
#9869 = CARTESIAN_POINT ( 'NONE',  ( -24.35964822603314772, 51.06041666571061199, -4.064049460664953983 ) ) ;
#9870 = CARTESIAN_POINT ( 'NONE',  ( 0.000000000000000000, 0.000000000000000000, 0.000000000000000000 ) ) ;
#9871 = CARTESIAN_POINT ( 'NONE',  ( -27.78268512908116961, 55.49961679590672503, -4.132201955500060642 ) ) ;
#9872 = AXIS2_PLACEMENT_3D ( 'NONE', #620, #4016, #5740 ) ;
#9873 = VERTEX_POINT ( 'NONE', #4865 ) ;
#9874 = CARTESIAN_POINT ( 'NONE',  ( -25.44486372867087809, 54.45623925897106687, -7.000000000000075495 ) ) ;
#9875 = CARTESIAN_POINT ( 'NONE',  ( -2.688821387764050996E-14, -4.618802153517012954, -0.4999999999999995559 ) ) ;
#9876 = ADVANCED_FACE ( 'NONE', ( #9971 ), #614, .T. ) ;
#9877 = EDGE_CURVE ( 'NONE', #8097, #10875, #10745, .T. ) ;
#9878 = DIRECTION ( 'NONE',  ( -1.000000000000000000, -0.000000000000000000, -0.000000000000000000 ) ) ;
#9879 = CARTESIAN_POINT ( 'NONE',  ( -27.60187600103308725, 53.51041666571062194, -5.935950539335252074 ) ) ;
#9880 = PRODUCT ( 'hex flange nut gradea_iso_ISO - 4161 - M5 - N', 'hex flange nut gradea_iso_ISO - 4161 - M5 - N', '', ( #1096 ) ) ;
#9881 = CARTESIAN_POINT ( 'NONE',  ( 19.95755123817951215, 17.62047157401400810, 12.00579112326941988 ) ) ;
#9882 =( BOUNDED_CURVE ( )  B_SPLINE_CURVE ( 1, ( #239, #3638 ),
 .UNSPECIFIED., .F., .T. ) 
 B_SPLINE_CURVE_WITH_KNOTS ( ( 2, 2 ),
 ( 0.000000000000000000, 1.000000000000000000 ),
 .UNSPECIFIED. ) 
 CURVE ( )  GEOMETRIC_REPRESENTATION_ITEM ( )  RATIONAL_B_SPLINE_CURVE ( ( 0.9343185842653825013, 0.9343185842653825013 ) ) 
 REPRESENTATION_ITEM ( '' )  );
#9883 = CARTESIAN_POINT ( 'NONE',  ( -26.79131905728310059, 54.85208333237729050, -6.403925809002825709 ) ) ;
#9884 = ORIENTED_EDGE ( 'NONE', *, *, #9586, .T. ) ;
#9885 = DIRECTION ( 'NONE',  ( 1.156482317317871478E-16, -0.000000000000000000, -1.000000000000000000 ) ) ;
#9886 = ORIENTED_EDGE ( 'NONE', *, *, #9732, .T. ) ;
#9887 = ORIENTED_EDGE ( 'NONE', *, *, #6540, .F. ) ;
#9888 = FACE_BOUND ( 'NONE', #317, .T. ) ;
#9889 = ORIENTED_EDGE ( 'NONE', *, *, #10142, .F. ) ;
#9890 = CARTESIAN_POINT ( 'NONE',  ( 2.500000000000008438, 30.00000000000000711, 15.84375000000000355 ) ) ;
#9891 =( NAMED_UNIT ( * ) SI_UNIT ( $, .STERADIAN. ) SOLID_ANGLE_UNIT ( ) );
#9892 = ORIENTED_EDGE ( 'NONE', *, *, #4860, .T. ) ;
#9894 = CARTESIAN_POINT ( 'NONE',  ( 22.93674656822681612, 23.24041807713223307, 10.95195840513859231 ) ) ;
#9893 = AXIS2_PLACEMENT_3D ( 'NONE', #8465, #9516, #10245 ) ;
#9895 = AXIS2_PLACEMENT_3D ( 'NONE', #2087, #6296, #5364 ) ;
#9896 = LINE ( 'NONE', #9009, #4413 ) ;
#9897 = CARTESIAN_POINT ( 'NONE',  ( 17.26579466391090634, 16.35877559204224951, 12.05147379044805866 ) ) ;
#9898 = CARTESIAN_POINT ( 'NONE',  ( -23.98076211353314235, 53.55416666475470322, -3.845299461620867554 ) ) ;
#9899 = VECTOR ( 'NONE', #3121, 1000.000000000000000 ) ;
#9900 = PRESENTATION_LAYER_ASSIGNMENT (  '', '', ( #3691 ) ) ;
#9901 = DIRECTION ( 'NONE',  ( 0.000000000000000000, 0.000000000000000000, 1.000000000000000000 ) ) ;
#9902 = CARTESIAN_POINT ( 'NONE',  ( -26.98076211353309972, 51.04583333142137036, -6.732050807568954909 ) ) ;
#9903 = ORIENTED_EDGE ( 'NONE', *, *, #3404, .T. ) ;
#9904 = VERTEX_POINT ( 'NONE', #4767 ) ;
#9905 = CARTESIAN_POINT ( 'NONE',  ( 16.39761867860600475, 18.55212878970134938, 13.19648031090924789 ) ) ;
#9906 = EDGE_CURVE ( 'NONE', #1521, #1617, #8300, .T. ) ;
#9907 = AXIS2_PLACEMENT_3D ( 'NONE', #10867, #4207, #5921 ) ;
#9908 = MECHANICAL_DESIGN_GEOMETRIC_PRESENTATION_REPRESENTATION (  '', ( #5654 ), #7939 ) ;
#9909 = CARTESIAN_POINT ( 'NONE',  ( 0.000000000000000000, 0.000000000000000000, -4.484454397937119197 ) ) ;
#9910 = CIRCLE ( 'NONE', #10974, 2.149999999999992362 ) ;
#9911 = CARTESIAN_POINT ( 'NONE',  ( 0.000000000000000000, 30.00000000000000000, -2.499999999999998668 ) ) ;
#9912 = CARTESIAN_POINT ( 'NONE',  ( -2.469212770973128190, 29.60886282244813827, 16.49922112211940117 ) ) ;
#9913 = CARTESIAN_POINT ( 'NONE',  ( -1.814555661125939912, 31.72097824480680117, 12.81469158473306713 ) ) ;
#9914 = DIRECTION ( 'NONE',  ( 0.000000000000000000, 0.000000000000000000, 1.000000000000000000 ) ) ;
#9915 = EDGE_LOOP ( 'NONE', ( #6965, #3892, #3143, #5438 ) ) ;
#9916 = CYLINDRICAL_SURFACE ( 'NONE', #7947, 1.999999999999971356 ) ;
#9917 = ORIENTED_EDGE ( 'NONE', *, *, #3348, .T. ) ;
#9918 = CARTESIAN_POINT ( 'NONE',  ( -1.101703131577911776, 27.52740819067395250, 15.20093341526694353 ) ) ;
#9919 = LINE ( 'NONE', #6569, #10056 ) ;
#9920 = CARTESIAN_POINT ( 'NONE',  ( 0.000000000000000000, 2.357898499370433054, -1.951563910473907981E-15 ) ) ;
#9921 = CARTESIAN_POINT ( 'NONE',  ( 3.200000000000000178, -4.041451884327390331, 2.328587628042611615E-14 ) ) ;
#9922 = CARTESIAN_POINT ( 'NONE',  ( 2.500000000000000000, 1.178949249685218525, 2.041999999999999371 ) ) ;
#9923 = CARTESIAN_POINT ( 'NONE',  ( -24.35964822603314417, 54.79374999904394627, -5.000000000000103029 ) ) ;
#9924 = CARTESIAN_POINT ( 'NONE',  ( 2.000000000000000000, 0.000000000000000000, 0.000000000000000000 ) ) ;
#9925 = DIRECTION ( 'NONE',  ( -1.000000000000000000, -0.000000000000000000, -0.000000000000000000 ) ) ;
#9926 = ORIENTED_EDGE ( 'NONE', *, *, #5161, .F. ) ;
#9927 = CARTESIAN_POINT ( 'NONE',  ( 2.474873734152918558, 32.47487373415292211, 14.75000000000000355 ) ) ;
#9928 = DIRECTION ( 'NONE',  ( 0.000000000000000000, 0.000000000000000000, 1.000000000000000000 ) ) ;
#9929 = EDGE_CURVE ( 'NONE', #10561, #5966, #9612, .T. ) ;
#9930 = CARTESIAN_POINT ( 'NONE',  ( -994.2085799786045754, 0.000000000000000000, 0.000000000000000000 ) ) ;
#9931 =( BOUNDED_SURFACE ( )  B_SPLINE_SURFACE ( 1, 2, ( 
 ( #7631, #6910, #6960, #8570, #10348, #844, #2691, #5140, #2641, #6017, #9402, #3625, #6066, #952, #4356, #3575, #123, #2744, #3467, #3524, #7747, #1849, #10297, #5243, #10405, #6118, #5302, #9513, #8687, #1062, #9287, #7854, #229, #1680, #5082, #5960, #8630, #7015, #5904, #1008, #179, #4420, #9348, #8460, #62, #6, #3407, #6849, #7805, #6788, #10183, #2577, #897, #4299, #7689, #10242, #5189, #9678, #4044, #6181, #9620, #7076, #1967, #1235, #2016, #5405, #3103, #2911, #6281, #1119, #5351, #6481, #4521, #8790, #2273, #4632, #7962, #2803, #1484, #1435, #7319, #339, #7376, #10762, #6229, #7428, #3682, #9569, #9883, #2073, #646, #10707, #1174, #8735, #10465, #5664, #7909, #9043, #4831, #4576, #8206, #3735, #287, #7122, #10517 ),
 ( #2859, #8016, #5460, #9934, #8851, #8262, #388, #3791, #586, #3982, #3154, #6537, #2319, #5711, #9090, #4882, #3203, #5762, #9377, #1773, #925, #10209, #4147, #6759, #7660, #8546, #4096, #2489, #4327, #8426, #870, #3438, #10989, #10818, #8316, #5049, #6582, #7541, #5874, #4271, #5822, #5164, #4214, #10929, #3260, #9985, #1543, #2369, #747, #6641, #8488, #697, #9146, #4995, #3321, #808, #4946, #7483, #10871, #10045, #2432, #2608, #6707, #10157, #35, #9204, #1597, #9258, #8368, #7604, #6813, #5986, #3379, #10102, #1652, #2544, #5926, #9314, #1711, #5110, #2719, #2043, #1089, #4447, #154, #3711, #8761, #7101, #5377, #93, #1144, #9649, #3493, #6877, #7776, #8709, #8824, #10494, #4497, #1991, #256, #3550, #4553, #1883, #9429 ) ),
 .UNSPECIFIED., .F., .F., .T. ) 
 B_SPLINE_SURFACE_WITH_KNOTS ( ( 2, 2 ),
 ( 3, 2, 2, 2, 2, 2, 2, 2, 2, 2, 2, 2, 2, 2, 2, 2, 2, 2, 2, 2, 2, 2, 2, 2, 2, 2, 2, 2, 2, 2, 2, 2, 2, 2, 2, 2, 2, 2, 2, 2, 2, 2, 2, 2, 2, 2, 2, 2, 2, 2, 2, 2, 3 ),
 ( 0.000000000000000000, 1.000000000000000000 ),
 ( 0.000000000000000000, 0.01851851851851851749, 0.03703703703703703498, 0.05555555555555555247, 0.07407407407407406996, 0.09259259259259258745, 0.1111111111111111049, 0.1296296296296296224, 0.1481481481481481399, 0.1666666666666666574, 0.1851851851851851749, 0.2037037037037036924, 0.2222222222222222099, 0.2407407407407407274, 0.2592592592592592449, 0.2777777777777777901, 0.2962962962962962798, 0.3148148148148148251, 0.3333333333333333148, 0.3518518518518518601, 0.3703703703703703498, 0.3888888888888888951, 0.4074074074074073848, 0.4259259259259259300, 0.4444444444444444198, 0.4629629629629629650, 0.4814814814814814548, 0.5000000000000000000, 0.5185185185185184897, 0.5370370370370370905, 0.5555555555555555802, 0.5740740740740740700, 0.5925925925925925597, 0.6111111111111111605, 0.6296296296296296502, 0.6481481481481481399, 0.6666666666666666297, 0.6851851851851852304, 0.7037037037037037202, 0.7222222222222222099, 0.7407407407407406996, 0.7592592592592593004, 0.7777777777777777901, 0.7962962962962962798, 0.8148148148148147696, 0.8333333333333333703, 0.8518518518518518601, 0.8703703703703703498, 0.8888888888888888395, 0.9074074074074074403, 0.9259259259259259300, 0.9444444444444444198, 0.9524110019352027834 ),
 .UNSPECIFIED. ) 
 GEOMETRIC_REPRESENTATION_ITEM ( )  RATIONAL_B_SPLINE_SURFACE ( (
 ( 1.000000000000000000, 0.8660254037844387076, 1.000000000000000000, 0.8660254037844387076, 1.000000000000000000, 0.8660254037844387076, 1.000000000000000000, 0.8660254037844387076, 1.000000000000000000, 0.8660254037844387076, 1.000000000000000000, 0.8660254037844387076, 1.000000000000000000, 0.8660254037844387076, 1.000000000000000000, 0.8660254037844387076, 1.000000000000000000, 0.8660254037844387076, 1.000000000000000000, 0.8660254037844387076, 1.000000000000000000, 0.8660254037844387076, 1.000000000000000000, 0.8660254037844387076, 1.000000000000000000, 0.8660254037844387076, 1.000000000000000000, 0.8660254037844387076, 1.000000000000000000, 0.8660254037844387076, 1.000000000000000000, 0.8660254037844387076, 1.000000000000000000, 0.8660254037844387076, 1.000000000000000000, 0.8660254037844387076, 1.000000000000000000, 0.8660254037844387076, 1.000000000000000000, 0.8660254037844387076, 1.000000000000000000, 0.8660254037844387076, 1.000000000000000000, 0.8660254037844387076, 1.000000000000000000, 0.8660254037844387076, 1.000000000000000000, 0.8660254037844387076, 1.000000000000000000, 0.8660254037844387076, 1.000000000000000000, 0.8660254037844387076, 1.000000000000000000, 0.8660254037844387076, 1.000000000000000000, 0.8660254037844387076, 1.000000000000000000, 0.8660254037844387076, 1.000000000000000000, 0.8660254037844387076, 1.000000000000000000, 0.8660254037844387076, 1.000000000000000000, 0.8660254037844387076, 1.000000000000000000, 0.8660254037844387076, 1.000000000000000000, 0.8660254037844387076, 1.000000000000000000, 0.8660254037844387076, 1.000000000000000000, 0.8660254037844387076, 1.000000000000000000, 0.8660254037844387076, 1.000000000000000000, 0.8660254037844387076, 1.000000000000000000, 0.8660254037844387076, 1.000000000000000000, 0.8660254037844387076, 1.000000000000000000, 0.8660254037844387076, 1.000000000000000000, 0.8660254037844387076, 1.000000000000000000, 0.8660254037844387076, 1.000000000000000000, 0.8660254037844387076, 1.000000000000000000, 0.8660254037844387076, 1.000000000000000000, 0.8660254037844387076, 1.000000000000000000, 0.8660254037844387076, 1.000000000000000000, 0.8660254037844387076, 1.000000000000000000, 0.8660254037844387076, 1.000000000000000000, 0.8660254037844387076, 1.000000000000000000, 0.8660254037844387076, 1.000000000000000000, 0.9423649185551699059, 0.9343183816103359796),
 ( 1.000000000000000000, 0.8660254037844387076, 1.000000000000000000, 0.8660254037844387076, 1.000000000000000000, 0.8660254037844387076, 1.000000000000000000, 0.8660254037844387076, 1.000000000000000000, 0.8660254037844387076, 1.000000000000000000, 0.8660254037844387076, 1.000000000000000000, 0.8660254037844387076, 1.000000000000000000, 0.8660254037844387076, 1.000000000000000000, 0.8660254037844387076, 1.000000000000000000, 0.8660254037844387076, 1.000000000000000000, 0.8660254037844387076, 1.000000000000000000, 0.8660254037844387076, 1.000000000000000000, 0.8660254037844387076, 1.000000000000000000, 0.8660254037844387076, 1.000000000000000000, 0.8660254037844387076, 1.000000000000000000, 0.8660254037844387076, 1.000000000000000000, 0.8660254037844387076, 1.000000000000000000, 0.8660254037844387076, 1.000000000000000000, 0.8660254037844387076, 1.000000000000000000, 0.8660254037844387076, 1.000000000000000000, 0.8660254037844387076, 1.000000000000000000, 0.8660254037844387076, 1.000000000000000000, 0.8660254037844387076, 1.000000000000000000, 0.8660254037844387076, 1.000000000000000000, 0.8660254037844387076, 1.000000000000000000, 0.8660254037844387076, 1.000000000000000000, 0.8660254037844387076, 1.000000000000000000, 0.8660254037844387076, 1.000000000000000000, 0.8660254037844387076, 1.000000000000000000, 0.8660254037844387076, 1.000000000000000000, 0.8660254037844387076, 1.000000000000000000, 0.8660254037844387076, 1.000000000000000000, 0.8660254037844387076, 1.000000000000000000, 0.8660254037844387076, 1.000000000000000000, 0.8660254037844387076, 1.000000000000000000, 0.8660254037844387076, 1.000000000000000000, 0.8660254037844387076, 1.000000000000000000, 0.8660254037844387076, 1.000000000000000000, 0.8660254037844387076, 1.000000000000000000, 0.8660254037844387076, 1.000000000000000000, 0.8660254037844387076, 1.000000000000000000, 0.8660254037844387076, 1.000000000000000000, 0.8660254037844387076, 1.000000000000000000, 0.8660254037844387076, 1.000000000000000000, 0.8660254037844387076, 1.000000000000000000, 0.8660254037844387076, 1.000000000000000000, 0.8660254037844387076, 1.000000000000000000, 0.8660254037844387076, 1.000000000000000000, 0.8660254037844387076, 1.000000000000000000, 0.8660254037844387076, 1.000000000000000000, 0.8660254037844387076, 1.000000000000000000, 0.9423649185551699059, 0.9343183816103359796) ) ) 
 REPRESENTATION_ITEM ( '' )  SURFACE ( )  );
#9932 = CARTESIAN_POINT ( 'NONE',  ( -25.98076211353310683, 53.39374999904394770, -6.871901078670399343 ) ) ;
#9933 = CARTESIAN_POINT ( 'NONE',  ( 19.83233192245754140, 21.00689442486442360, 11.00732503135576401 ) ) ;
#9934 = CARTESIAN_POINT ( 'NONE',  ( -25.98076211353311393, 49.67499999999986926, -7.309401076758571314 ) ) ;
#9935 = ORIENTED_EDGE ( 'NONE', *, *, #1289, .T. ) ;
#9936 = ADVANCED_FACE ( 'NONE', ( #8979 ), #3118, .T. ) ;
#9937 = CARTESIAN_POINT ( 'NONE',  ( -27.60187600103308014, 55.20208333237728482, -4.064049460664955760 ) ) ;
#9938 = ORIENTED_EDGE ( 'NONE', *, *, #4527, .T. ) ;
#9939 = ORIENTED_EDGE ( 'NONE', *, *, #553, .F. ) ;
#9940 = CARTESIAN_POINT ( 'NONE',  ( 2.500000000000000000, -2.357898499370432610, 3.252606517456513302E-15 ) ) ;
#9941 = ORIENTED_EDGE ( 'NONE', *, *, #8232, .F. ) ;
#9942 = EDGE_CURVE ( 'NONE', #2863, #4665, #6129, .T. ) ;
#9943 = FACE_OUTER_BOUND ( 'NONE', #9591, .T. ) ;
#9944 = ORIENTED_EDGE ( 'NONE', *, *, #5536, .F. ) ;
#9945 = CARTESIAN_POINT ( 'NONE',  ( 17.16312581766332457, 17.78662165064481471, 11.12029599681952519 ) ) ;
#9946 = DIRECTION ( 'NONE',  ( 0.000000000000000000, -1.000000000000000000, 0.000000000000000000 ) ) ;
#9947 =( BOUNDED_CURVE ( )  B_SPLINE_CURVE ( 2, ( #7712, #3490, #2717, #4268, #6872, #980, #5162, #4323, #10264 ),
 .UNSPECIFIED., .F., .F. ) 
 B_SPLINE_CURVE_WITH_KNOTS ( ( 3, 2, 2, 2, 3 ),
 ( 0.1944444444444444475, 0.2037037037037036924, 0.2222222222222222099, 0.2407407407407407274, 0.2500000000000000000 ),
 .UNSPECIFIED. ) 
 CURVE ( )  GEOMETRIC_REPRESENTATION_ITEM ( )  RATIONAL_B_SPLINE_CURVE ( ( 0.9330127018922192983, 0.9330127018922194093, 1.000000000000000000, 0.8660254037844387076, 1.000000000000000000, 0.8660254037844387076, 1.000000000000000000, 0.9330127018922191873, 0.9330127018922192983 ) ) 
 REPRESENTATION_ITEM ( '' )  );
#9948 = CARTESIAN_POINT ( 'NONE',  ( 0.5469614295415388128, -4.303013824935362663, -3.535263753543555598 ) ) ;
#9949 = CARTESIAN_POINT ( 'NONE',  ( 18.07012887690021330, 16.02595819568259827, 12.00212024154935975 ) ) ;
#9950 = EDGE_CURVE ( 'NONE', #7325, #2956, #7685, .T. ) ;
#9951 = CARTESIAN_POINT ( 'NONE',  ( -24.98076211353312814, 51.62916666475469896, -6.732050807568954909 ) ) ;
#9952 = CARTESIAN_POINT ( 'NONE',  ( 34.80704760714191082, 3.674543421742910709, -2.801642449272108593 ) ) ;
#9953 = ORIENTED_EDGE ( 'NONE', *, *, #7491, .F. ) ;
#9954 = CARTESIAN_POINT ( 'NONE',  ( -2.474873734152920335, 32.47487373415291501, 13.81250000000000355 ) ) ;
#9955 = ORIENTED_EDGE ( 'NONE', *, *, #2409, .T. ) ;
#9956 = ADVANCED_FACE ( 'NONE', ( #187 ), #2528, .F. ) ;
#9957 = EDGE_CURVE ( 'NONE', #101, #2436, #8315, .T. ) ;
#9958 = CARTESIAN_POINT ( 'NONE',  ( 21.04196501824306864, 22.63405165899350635, 13.00425721518307753 ) ) ;
#9959 = CONICAL_SURFACE ( 'NONE', #4287, 4.000000000000000000, 0.8911886515913786111 ) ;
#9960 = LINE ( 'NONE', #8962, #10218 ) ;
#9961 = DIRECTION ( 'NONE',  ( 0.000000000000000000, 1.000000000000000000, 0.000000000000000000 ) ) ;
#9962 = CYLINDRICAL_SURFACE ( 'NONE', #5537, 1.999999999999971356 ) ;
#9963 = CARTESIAN_POINT ( 'NONE',  ( 0.06616922564517943584, 27.49999999999998934, 14.53344158473306535 ) ) ;
#9964 = CARTESIAN_POINT ( 'NONE',  ( -23.98076211353314235, 51.57083333142138315, -6.154700538379337615 ) ) ;
#9965 = ORIENTED_EDGE ( 'NONE', *, *, #8723, .T. ) ;
#9966 = CARTESIAN_POINT ( 'NONE',  ( -21.21106610644865498, 13.49999999999941913, -9.500000000000000000 ) ) ;
#9967 = EDGE_LOOP ( 'NONE', ( #10665, #8265, #3261, #9044 ) ) ;
#9968 = CARTESIAN_POINT ( 'NONE',  ( 1.383578242660662871, 26.47259180932604039, 15.35718341526694530 ) ) ;
#9969 = CARTESIAN_POINT ( 'NONE',  ( 24.55500000000002103, 3.061616997868384620E-16, -2.500000000000001332 ) ) ;
#9970 = CARTESIAN_POINT ( 'NONE',  ( -24.98076211353313170, 52.09583333142136752, -3.267949192431250705 ) ) ;
#9971 = FACE_OUTER_BOUND ( 'NONE', #5613, .T. ) ;
#9972 = EDGE_CURVE ( 'NONE', #3779, #7151, #10392, .T. ) ;
#9973 = CARTESIAN_POINT ( 'NONE',  ( -2.100000000000000089, 2.571758278209441957E-16, -5.000000000000000000 ) ) ;
#9974 = CARTESIAN_POINT ( 'NONE',  ( -27.44132332507749439, 55.89336679508493688, -4.296600267573891685 ) ) ;
#9975 = CARTESIAN_POINT ( 'NONE',  ( 3.061857526609965685, -1.355358988605187998, 3.499999999999999556 ) ) ;
#9976 = CARTESIAN_POINT ( 'NONE',  ( 4.000000000000000888, -0.8578082829538523635, -3.433262215449808696 ) ) ;
#9977 = ORIENTED_EDGE ( 'NONE', *, *, #7287, .T. ) ;
#9978 = CARTESIAN_POINT ( 'NONE',  ( 2.474873734152922111, 27.52512626584708144, 14.43750000000000178 ) ) ;
#9979 = VECTOR ( 'NONE', #6932, 1000.000000000000000 ) ;
#9980 = CARTESIAN_POINT ( 'NONE',  ( -2.100000000000000089, 2.571758278209441957E-16, -0.2800830152838844622 ) ) ;
#9981 = CARTESIAN_POINT ( 'NONE',  ( -27.60187600103308725, 50.88541666571061484, -5.935950539335252074 ) ) ;
#9982 = CARTESIAN_POINT ( 'NONE',  ( -24.35964822603314772, 52.46041666571062478, -4.064049460664953983 ) ) ;
#9983 = EDGE_CURVE ( 'NONE', #2646, #2508, #8818, .T. ) ;
#9984 = CARTESIAN_POINT ( 'NONE',  ( 20.21677217982034946, 21.95921345637081501, 11.00732503135595941 ) ) ;
#9985 = CARTESIAN_POINT ( 'NONE',  ( -25.98076211353311393, 52.12499999999986500, -2.690598923241634743 ) ) ;
#9986 = ORIENTED_EDGE ( 'NONE', *, *, #6882, .T. ) ;
#9987 = CARTESIAN_POINT ( 'NONE',  ( 2.982579934988325743, -2.185595227305077604, -3.214438021527616929 ) ) ;
#9988 = VERTEX_POINT ( 'NONE', #6689 ) ;
#9989 = ORIENTED_EDGE ( 'NONE', *, *, #7672, .F. ) ;
#9990 = FACE_OUTER_BOUND ( 'NONE', #7429, .T. ) ;
#9991 = EDGE_LOOP ( 'NONE', ( #6235, #5262, #7275, #450, #7821, #10394 ) ) ;
#9992 = CARTESIAN_POINT ( 'NONE',  ( 2.500000000000000000, 1.178949249685213863, -2.042000000000001148 ) ) ;
#9993 = ORIENTED_EDGE ( 'NONE', *, *, #20, .T. ) ;
#9994 = CARTESIAN_POINT ( 'NONE',  ( 22.42490604353609029, 22.35994869845890065, 11.00732503135576401 ) ) ;
#9995 =( NAMED_UNIT ( * ) SI_UNIT ( $, .STERADIAN. ) SOLID_ANGLE_UNIT ( ) );
#9996 = CARTESIAN_POINT ( 'NONE',  ( 30.75045812061784289, 53.49999999999983658, 10.00000000000000178 ) ) ;
#9997 = CARTESIAN_POINT ( 'NONE',  ( -24.35964822603314417, 49.89374999904394770, -5.000000000000103029 ) ) ;
#9998 = EDGE_CURVE ( 'NONE', #2160, #9093, #4197, .T. ) ;
#9999 = CARTESIAN_POINT ( 'NONE',  ( 19.93275388331568365, 16.31952634560019888, 12.94889180291853492 ) ) ;
#10000 = CARTESIAN_POINT ( 'NONE',  ( -24.98076211353313170, 52.79583333142137036, -3.267949192431250705 ) ) ;
#10001 = CARTESIAN_POINT ( 'NONE',  ( 29.50000000000000711, 1.799097979968134709E-15, 2.500000000000000000 ) ) ;
#10002 = LINE ( 'NONE', #7391, #10438 ) ;
#10003 = PRODUCT_DEFINITION_CONTEXT ( 'detailed design', #5515, 'design' ) ;
#10004 = ORIENTED_EDGE ( 'NONE', *, *, #2602, .T. ) ;
#10005 = CARTESIAN_POINT ( 'NONE',  ( -2.521662442312483599, 27.57191497400664204, 16.37280841526694175 ) ) ;
#10006 = EDGE_LOOP ( 'NONE', ( #8768, #1134, #10534, #247 ) ) ;
#10007 = CARTESIAN_POINT ( 'NONE',  ( 22.67082259973814828, 19.44041185113230341, 13.00425721518326938 ) ) ;
#10008 = EDGE_CURVE ( 'NONE', #2222, #2458, #10141, .T. ) ;
#10009 = EDGE_CURVE ( 'NONE', #4732, #6093, #297, .T. ) ;
#10010 = CARTESIAN_POINT ( 'NONE',  ( 11.61000000000001542, 0.000000000000000000, 0.000000000000000000 ) ) ;
#10011 = CARTESIAN_POINT ( 'NONE',  ( -25.98076211353311393, 50.02499999999987068, -3.000000000000132783 ) ) ;
#10012 = CARTESIAN_POINT ( 'NONE',  ( -26.11503144744077076, 56.99999999999888445, -3.000000000000131894 ) ) ;
#10013 = CIRCLE ( 'NONE', #3637, 2.000000000000000000 ) ;
#10014 = CLOSED_SHELL ( 'NONE', ( #10635, #7344, #8595, #6799, #915, #1751, #165, #7119, #6683, #6164, #10814, #3716, #2752, #10426, #5348, #1658, #3910, #10294, #7944, #1256, #3895, #488, #8128, #7802, #3149, #9111, #1572, #608, #3928, #10080, #1005, #2418, #9605, #4571 ) ) ;
#10015 = CARTESIAN_POINT ( 'NONE',  ( -2.428085025993349078, 27.47833755768751374, 14.37719158473306713 ) ) ;
#10016 = DIRECTION ( 'NONE',  ( -1.000000000000000000, 0.000000000000000000, -0.000000000000000000 ) ) ;
#10017 = AXIS2_PLACEMENT_3D ( 'NONE', #4054, #9097, #1492 ) ;
#10018 = PLANE ( 'NONE',  #3639 ) ;
#10019 = CARTESIAN_POINT ( 'NONE',  ( 3.078243469714883940, -3.710888496608934606, -0.5725525826504437310 ) ) ;
#10020 = ORIENTED_EDGE ( 'NONE', *, *, #4597, .F. ) ;
#10021 = VERTEX_POINT ( 'NONE', #1300 ) ;
#10022 = DIRECTION ( 'NONE',  ( 1.000000000000000000, 0.000000000000000000, 0.000000000000000000 ) ) ;
#10023 = AXIS2_PLACEMENT_3D ( 'NONE', #5227, #6827, #10170 ) ;
#10024 = CARTESIAN_POINT ( 'NONE',  ( -25.98076211353311393, 53.17499999999985505, -7.000000000000072831 ) ) ;
#10025 = AXIS2_PLACEMENT_3D ( 'NONE', #10888, #3280, #8506 ) ;
#10026 = CARTESIAN_POINT ( 'NONE',  ( 17.86810043078960319, 17.16701444005803268, 12.06109941161078325 ) ) ;
#10027 = AXIS2_PLACEMENT_3D ( 'NONE', #2253, #7466, #9075 ) ;
#10028 = VECTOR ( 'NONE', #4560, 1000.000000000000000 ) ;
#10029 = LINE ( 'NONE', #5747, #1881 ) ;
#10030 = FACE_BOUND ( 'NONE', #3672, .T. ) ;
#10031 = CARTESIAN_POINT ( 'NONE',  ( -25.98076211353311393, 54.96874999904394343, -6.871901078670400231 ) ) ;
#10032 = DIRECTION ( 'NONE',  ( 0.000000000000000000, 1.000000000000000000, 0.000000000000000000 ) ) ;
#10033 = CARTESIAN_POINT ( 'NONE',  ( -24.35964822603314417, 49.89374999904394770, -5.000000000000103029 ) ) ;
#10034 = AXIS2_PLACEMENT_3D ( 'NONE', #722, #7510, #10958 ) ;
#10035 = ORIENTED_EDGE ( 'NONE', *, *, #6280, .T. ) ;
#10036 = CARTESIAN_POINT ( 'NONE',  ( -3.500000000000003997, 31.44974746830583001, 13.89062500000000355 ) ) ;
#10037 = AXIS2_PLACEMENT_3D ( 'NONE', #2709, #7820, #6978 ) ;
#10038 = DIRECTION ( 'NONE',  ( 0.000000000000000000, 0.000000000000000000, -1.000000000000000000 ) ) ;
#10039 = DIRECTION ( 'NONE',  ( 0.000000000000000000, 0.000000000000000000, -1.000000000000000000 ) ) ;
#10040 = DIRECTION ( 'NONE',  ( 0.000000000000000000, -0.000000000000000000, 1.000000000000000000 ) ) ;
#10041 = EDGE_CURVE ( 'NONE', #6804, #3990, #7196, .T. ) ;
#10042 = CARTESIAN_POINT ( 'NONE',  ( -25.98076211353310683, 54.09374999904395054, -6.871901078670399343 ) ) ;
#10043 = AXIS2_PLACEMENT_3D ( 'NONE', #6128, #5252, #2020 ) ;
#10044 = CARTESIAN_POINT ( 'NONE',  ( 20.17304365239387565, 21.99495017005343200, 12.00579112326981068 ) ) ;
#10045 = CARTESIAN_POINT ( 'NONE',  ( -23.98076211353314235, 52.94166666666653498, -3.845299461620867554 ) ) ;
#10046 = ORIENTED_EDGE ( 'NONE', *, *, #8671, .T. ) ;
#10047 = APPLICATION_CONTEXT ( 'automotive_design' ) ;
#10048 = CARTESIAN_POINT ( 'NONE',  ( 0.000000000000000000, 0.000000000000000000, -5.000000000000000000 ) ) ;
#10049 = ORIENTED_EDGE ( 'NONE', *, *, #1433, .F. ) ;
#10050 = VERTEX_POINT ( 'NONE', #2867 ) ;
#10051 = CYLINDRICAL_SURFACE ( 'NONE', #959, 2.999999999999999112 ) ;
#10052 = ORIENTED_EDGE ( 'NONE', *, *, #2147, .F. ) ;
#10053 = CARTESIAN_POINT ( 'NONE',  ( 2.650000000000095834, 30.00000000000000000, 2.500000000000000000 ) ) ;
#10054 = DIRECTION ( 'NONE',  ( 0.000000000000000000, 0.000000000000000000, 1.000000000000000000 ) ) ;
#10055 = EDGE_LOOP ( 'NONE', ( #9830, #5631, #2145, #5993, #4690 ) ) ;
#10056 = VECTOR ( 'NONE', #9865, 1000.000000000000000 ) ;
#10057 = CARTESIAN_POINT ( 'NONE',  ( 17.08513846059531005, 17.86460900771146143, 11.12760988119559258 ) ) ;
#10058 = SURFACE_SIDE_STYLE ('',( #2446 ) ) ;
#10059 = DIRECTION ( 'NONE',  ( -0.5735764363510461594, 0.000000000000000000, 0.8191520442889916875 ) ) ;
#10060 = CARTESIAN_POINT ( 'NONE',  ( 16.19085831639751305, 17.34467558953444311, 12.14735994959144350 ) ) ;
#10061 = CARTESIAN_POINT ( 'NONE',  ( -23.98076211353314235, 54.31249999808803608, -5.000000000000103029 ) ) ;
#10062 = CARTESIAN_POINT ( 'NONE',  ( 3.319999999999999840, 4.127059713126577826E-16, 3.369999999999997886 ) ) ;
#10063 = VERTEX_POINT ( 'NONE', #1185 ) ;
#10064 = PLANE ( 'NONE',  #483 ) ;
#10065 = ORIENTED_EDGE ( 'NONE', *, *, #4190, .T. ) ;
#10066 = AXIS2_PLACEMENT_3D ( 'NONE', #8019, #391, #2914 ) ;
#10067 = CARTESIAN_POINT ( 'NONE',  ( -2.505208318772514708, 29.86938897312880314, 17.48140433884295319 ) ) ;
#10068 = VERTEX_POINT ( 'NONE', #4695 ) ;
#10069 = ADVANCED_FACE ( 'NONE', ( #3745 ), #6972, .T. ) ;
#10070 = CARTESIAN_POINT ( 'NONE',  ( 16.08167231043895384, 17.45386159549338245, 13.15979613361243494 ) ) ;
#10071 = CARTESIAN_POINT ( 'NONE',  ( 21.04731615659443733, 17.16224689484156585, 11.95042449705224819 ) ) ;
#10072 = CIRCLE ( 'NONE', #6698, 0.4999999999999985567 ) ;
#10073 = CIRCLE ( 'NONE', #484, 0.4999999999999981681 ) ;
#10074 = FACE_OUTER_BOUND ( 'NONE', #10737, .T. ) ;
#10075 = CARTESIAN_POINT ( 'NONE',  ( 2.887392608830347207, 2.020725942163738686, 3.499999999999999556 ) ) ;
#10076 = CARTESIAN_POINT ( 'NONE',  ( 2.428085025993350410, 32.52166244231248271, 13.75219158473306535 ) ) ;
#10077 = DIRECTION ( 'NONE',  ( -0.000000000000000000, -0.000000000000000000, 1.000000000000000000 ) ) ;
#10078 = VERTEX_POINT ( 'NONE', #4530 ) ;
#10079 = FACE_OUTER_BOUND ( 'NONE', #753, .T. ) ;
#10080 = ADVANCED_FACE ( 'NONE', ( #10360 ), #7132, .F. ) ;
#10081 = EDGE_LOOP ( 'NONE', ( #9392, #10179, #9582 ) ) ;
#10082 = EDGE_LOOP ( 'NONE', ( #4294, #621, #5508, #7694 ) ) ;
#10083 =( GEOMETRIC_REPRESENTATION_CONTEXT ( 3 ) GLOBAL_UNCERTAINTY_ASSIGNED_CONTEXT ( ( #1436 ) ) GLOBAL_UNIT_ASSIGNED_CONTEXT ( ( #6013, #6845, #8516 ) ) REPRESENTATION_CONTEXT ( 'NONE', 'WORKASPACE' ) );
#10084 = CARTESIAN_POINT ( 'NONE',  ( -27.98076211353308551, 52.00833333333319786, -3.845299461620869330 ) ) ;
#10085 = LINE ( 'NONE', #1757, #10939 ) ;
#10086 = PRESENTATION_LAYER_ASSIGNMENT (  '', '', ( #855 ) ) ;
#10087 = CARTESIAN_POINT ( 'NONE',  ( 0.000000000000000000, 0.000000000000000000, 0.000000000000000000 ) ) ;
#10088 = CARTESIAN_POINT ( 'NONE',  ( 2.500000000000010214, 28.96446609406726580, 14.51562500000000355 ) ) ;
#10089 = DIRECTION ( 'NONE',  ( 0.5150380749100551547, 0.000000000000000000, -0.8571673007021116675 ) ) ;
#10090 = CARTESIAN_POINT ( 'NONE',  ( -25.98076211353311393, 51.29374999904394627, -6.871901078670400231 ) ) ;
#10091 = FACE_OUTER_BOUND ( 'NONE', #6434, .T. ) ;
#10092 = COLOUR_RGB ( '', 0.09019608, 0.27058824, 0.51372549) ;
#10093 = CARTESIAN_POINT ( 'NONE',  ( 30.75045812061784289, 56.49999999999984368, 2.500000000000000000 ) ) ;
#10094 = ADVANCED_FACE ( 'NONE', ( #9577 ), #7973, .F. ) ;
#10095 = ORIENTED_EDGE ( 'NONE', *, *, #5861, .T. ) ;
#10096 = AXIS2_PLACEMENT_3D ( 'NONE', #6561, #4183, #3352 ) ;
#10097 = LINE ( 'NONE', #5101, #420 ) ;
#10098 = DIRECTION ( 'NONE',  ( 1.000000000000000000, -0.000000000000000000, 1.156482317317871478E-16 ) ) ;
#10099 = EDGE_CURVE ( 'NONE', #2929, #2222, #2083, .T. ) ;
#10100 = CARTESIAN_POINT ( 'NONE',  ( -25.98076211353310683, 54.26874999904394059, -6.871901078670399343 ) ) ;
#10101 = CARTESIAN_POINT ( 'NONE',  ( -24.35964822603314772, 52.57708333237728482, -5.935950539335252074 ) ) ;
#10102 = CARTESIAN_POINT ( 'NONE',  ( -23.98076211353314235, 53.75833333333319786, -6.154700538379337615 ) ) ;
#10103 = ORIENTED_EDGE ( 'NONE', *, *, #358, .F. ) ;
#10104 = VERTEX_POINT ( 'NONE', #6293 ) ;
#10106 = VERTEX_POINT ( 'NONE', #1127 ) ;
#10105 = EDGE_CURVE ( 'NONE', #3014, #3474, #6534, .T. ) ;
#10107 = DIRECTION ( 'NONE',  ( -0.000000000000000000, -0.000000000000000000, 1.000000000000000000 ) ) ;
#10108 = ORIENTED_EDGE ( 'NONE', *, *, #3715, .F. ) ;
#10109 = DIRECTION ( 'NONE',  ( 0.000000000000000000, 0.000000000000000000, -1.000000000000000000 ) ) ;
#10110 = DIRECTION ( 'NONE',  ( -1.000000000000000000, -7.997609853289037444E-17, 1.368128411675315488E-17 ) ) ;
#10111 = ORIENTED_EDGE ( 'NONE', *, *, #624, .F. ) ;
#10112 = CARTESIAN_POINT ( 'NONE',  ( 20.44553565182888732, 18.02736169756263962, 11.00732503135576401 ) ) ;
#10113 = CARTESIAN_POINT ( 'NONE',  ( -4.000000000000000000, 0.1981133338132459731, 2.096406544454392723E-17 ) ) ;
#10114 = CARTESIAN_POINT ( 'NONE',  ( -25.98076211353311038, 61.49999999999985789, -9.000000000000701661 ) ) ;
#10115 = CARTESIAN_POINT ( 'NONE',  ( 23.94195266346560658, 19.36439822498074648, 12.94889058896590583 ) ) ;
#10116 = DIRECTION ( 'NONE',  ( -0.000000000000000000, -0.000000000000000000, -1.000000000000000000 ) ) ;
#10117 = CARTESIAN_POINT ( 'NONE',  ( -24.98076211353312814, 55.12916666475470606, -6.732050807568954909 ) ) ;
#10118 = DIRECTION ( 'NONE',  ( 1.000000000000000000, 0.000000000000000000, 0.000000000000000000 ) ) ;
#10119 = ORIENTED_EDGE ( 'NONE', *, *, #1270, .T. ) ;
#10120 = DIRECTION ( 'NONE',  ( -0.000000000000000000, -0.000000000000000000, 1.000000000000000000 ) ) ;
#10121 = ORIENTED_EDGE ( 'NONE', *, *, #5933, .T. ) ;
#10122 = CARTESIAN_POINT ( 'NONE',  ( -3.500000000000003553, 31.44974746830583356, 15.14062500000000355 ) ) ;
#10123 = EDGE_LOOP ( 'NONE', ( #8403, #3268, #539 ) ) ;
#10124 = CARTESIAN_POINT ( 'NONE',  ( 22.11813463801259161, 17.83967204375498383, 12.94889058896590583 ) ) ;
#10125 = DIRECTION ( 'NONE',  ( 0.000000000000000000, 1.000000000000000000, 0.000000000000000000 ) ) ;
#10126 = LINE ( 'NONE', #1512, #9198 ) ;
#10127 = LINE ( 'NONE', #2466, #4106 ) ;
#10128 = EDGE_CURVE ( 'NONE', #10904, #2973, #3588, .T. ) ;
#10129 = CARTESIAN_POINT ( 'NONE',  ( -1.035533905932742638, 32.50000000000000000, 14.98437500000000711 ) ) ;
#10130 = CARTESIAN_POINT ( 'NONE',  ( 0.000000000000000000, 0.000000000000000000, 3.469446951953614189E-15 ) ) ;
#10131 = CARTESIAN_POINT ( 'NONE',  ( 0.000000000000000000, 0.000000000000000000, -2.500000000000000000 ) ) ;
#10132 = DIRECTION ( 'NONE',  ( -0.000000000000000000, 1.000000000000000000, -0.000000000000000000 ) ) ;
#10133 = B_SPLINE_CURVE_WITH_KNOTS ( 'NONE', 3,
 ( #3411, #4361, #2469, #64, #5907, #5191 ),
 .UNSPECIFIED., .F., .F.,
 ( 4, 2, 4 ),
 ( 0.002044882221487562268, 0.003063384235218290751, 0.004081886248949019233 ),
 .UNSPECIFIED. ) ;
#10134 = VERTEX_POINT ( 'NONE', #4483 ) ;
#10135 = EDGE_LOOP ( 'NONE', ( #1993, #2204, #5929, #2710 ) ) ;
#10136 = FACE_OUTER_BOUND ( 'NONE', #3739, .T. ) ;
#10137 = VECTOR ( 'NONE', #5748, 1000.000000000000000 ) ;
#10138 = DIRECTION ( 'NONE',  ( 0.8660254037844379305, 0.5000000000000013323, 0.000000000000000000 ) ) ;
#10139 = CARTESIAN_POINT ( 'NONE',  ( 20.23853826540680600, 19.71164639310234534, 12.00579112326941988 ) ) ;
#10140 = PRODUCT_DEFINITION ( 'UNKNOWN', '', #125, #6666 ) ;
#10141 = LINE ( 'NONE', #7085, #3292 ) ;
#10142 = EDGE_CURVE ( 'NONE', #2370, #8872, #825, .T. ) ;
#10143 = FACE_OUTER_BOUND ( 'NONE', #9293, .T. ) ;
#10144 = CARTESIAN_POINT ( 'NONE',  ( -26.79131905728310059, 55.08541666571061768, -3.596074190997381237 ) ) ;
#10145 = ADVANCED_FACE ( 'NONE', ( #7184 ), #7867, .T. ) ;
#10146 = FACE_OUTER_BOUND ( 'NONE', #9368, .T. ) ;
#10147 = DIRECTION ( 'NONE',  ( 0.000000000000000000, 0.000000000000000000, 1.000000000000000000 ) ) ;
#10148 = CARTESIAN_POINT ( 'NONE',  ( 4.000000000000000000, 2.309401076758515803, -0.4999999999999995559 ) ) ;
#10149 = VERTEX_POINT ( 'NONE', #2816 ) ;
#10150 = FACE_OUTER_BOUND ( 'NONE', #10411, .T. ) ;
#10151 = FACE_BOUND ( 'NONE', #4784, .T. ) ;
#10152 = CARTESIAN_POINT ( 'NONE',  ( -25.98076211353310683, 52.51874999904394770, -3.128098921329806714 ) ) ;
#10153 = EDGE_CURVE ( 'NONE', #1456, #10839, #2023, .T. ) ;
#10154 = DIRECTION ( 'NONE',  ( 0.000000000000000000, 0.000000000000000000, 1.000000000000000000 ) ) ;
#10155 = EDGE_CURVE ( 'NONE', #7809, #9774, #9882, .T. ) ;
#10156 = FACE_OUTER_BOUND ( 'NONE', #3795, .T. ) ;
#10157 = CARTESIAN_POINT ( 'NONE',  ( -25.98076211353311393, 53.17499999999985505, -7.309401076758571314 ) ) ;
#10158 = VECTOR ( 'NONE', #255, 1000.000000000000000 ) ;
#10159 = VERTEX_POINT ( 'NONE', #8074 ) ;
#10160 = ORIENTED_EDGE ( 'NONE', *, *, #2542, .T. ) ;
#10161 = ORIENTED_EDGE ( 'NONE', *, *, #761, .F. ) ;
#10162 = DIRECTION ( 'NONE',  ( 0.000000000000000000, 0.000000000000000000, -1.000000000000000000 ) ) ;
#10163 = ORIENTED_EDGE ( 'NONE', *, *, #10486, .T. ) ;
#10164 = CARTESIAN_POINT ( 'NONE',  ( 0.000000000000000000, 2.357898499370433054, -1.951563910473907981E-15 ) ) ;
#10165 = DIRECTION ( 'NONE',  ( 1.387778780781445213E-17, -8.326672684688671588E-17, -0.9999999999999998890 ) ) ;
#10166 = ORIENTED_EDGE ( 'NONE', *, *, #9415, .T. ) ;
#10167 = CARTESIAN_POINT ( 'NONE',  ( 23.26254143866440671, 20.58647472722595850, 11.00732503135576401 ) ) ;
#10168 = CARTESIAN_POINT ( 'NONE',  ( -25.98076211353311393, 55.27499999999985647, -7.000000000000072831 ) ) ;
#10169 = VECTOR ( 'NONE', #1901, 1000.000000000000227 ) ;
#10170 = DIRECTION ( 'NONE',  ( -1.000000000000000000, 0.000000000000000000, 0.000000000000000000 ) ) ;
#10171 = CARTESIAN_POINT ( 'NONE',  ( 3.170065989602867340, -3.373851915354596720, 1.156317065392270749 ) ) ;
#10172 = CARTESIAN_POINT ( 'NONE',  ( 15.12656308325174415, 18.40897082268132934, 11.24497629747462568 ) ) ;
#10173 = DIRECTION ( 'NONE',  ( 1.000000000000000000, -0.000000000000000000, 1.156482317317871478E-16 ) ) ;
#10174 = CARTESIAN_POINT ( 'NONE',  ( -25.98076211353311393, 54.48749999808803324, -7.309401076758571314 ) ) ;
#10175 = ORIENTED_EDGE ( 'NONE', *, *, #9496, .F. ) ;
#10176 = DIRECTION ( 'NONE',  ( 0.000000000000000000, 0.000000000000000000, -1.000000000000000000 ) ) ;
#10177 = ORIENTED_EDGE ( 'NONE', *, *, #10452, .F. ) ;
#10178 = CARTESIAN_POINT ( 'NONE',  ( -3.500000000000001332, 29.93383077435482065, 15.47094158473306535 ) ) ;
#10179 = ORIENTED_EDGE ( 'NONE', *, *, #7811, .F. ) ;
#10180 = CARTESIAN_POINT ( 'NONE',  ( 23.39622245855813176, 20.94697541805627239, 13.00425721518248956 ) ) ;
#10181 = DIRECTION ( 'NONE',  ( 0.000000000000000000, -0.4999999999999991118, 0.8660254037844391517 ) ) ;
#10182 = CARTESIAN_POINT ( 'NONE',  ( 22.11805565807571128, 22.55986279155152374, 12.00579112326941988 ) ) ;
#10183 = CARTESIAN_POINT ( 'NONE',  ( -25.17020516978313083, 52.63541666571061484, -6.403925809002825709 ) ) ;
#10184 = CARTESIAN_POINT ( 'NONE',  ( 1.767766952966377314, 28.23223304703363112, 15.68750000000000355 ) ) ;
#10185 = DIRECTION ( 'NONE',  ( 0.000000000000000000, -0.8660254037844317132, 0.5000000000000122125 ) ) ;
#10186 = CARTESIAN_POINT ( 'NONE',  ( 3.469446951953614189E-15, -1.040834085586084257E-14, -2.500000000000000000 ) ) ;
#10187 = LINE ( 'NONE', #5964, #4399 ) ;
#10188 = ORIENTED_EDGE ( 'NONE', *, *, #1272, .F. ) ;
#10189 = ORIENTED_EDGE ( 'NONE', *, *, #2856, .F. ) ;
#10190 = AXIS2_PLACEMENT_3D ( 'NONE', #1151, #4663, #157 ) ;
#10191 = CARTESIAN_POINT ( 'NONE',  ( 5.000000000000004441, 0.000000000000000000, 0.000000000000000000 ) ) ;
#10192 = DIRECTION ( 'NONE',  ( 0.5000000000000013323, -0.8660254037844379305, 0.000000000000000000 ) ) ;
#10193 = CARTESIAN_POINT ( 'NONE',  ( 21.90605485701305000, 18.97586566459109392, 12.00579112326941988 ) ) ;
#10194 = CARTESIAN_POINT ( 'NONE',  ( 1.767766952966377314, 28.23223304703363112, 15.68750000000000355 ) ) ;
#10195 = CARTESIAN_POINT ( 'NONE',  ( -25.98076211353311393, 52.47499999999985931, -7.000000000000072831 ) ) ;
#10196 = CARTESIAN_POINT ( 'NONE',  ( -25.17020516978313083, 51.93541666571061910, -6.403925809002825709 ) ) ;
#10197 = CIRCLE ( 'NONE', #8233, 0.2000000000000000944 ) ;
#10198 = DIRECTION ( 'NONE',  ( 1.156482317317871478E-16, -1.807003620809174139E-16, -1.000000000000000000 ) ) ;
#10199 = FACE_OUTER_BOUND ( 'NONE', #5716, .T. ) ;
#10200 = FACE_OUTER_BOUND ( 'NONE', #9832, .T. ) ;
#10201 = VERTEX_POINT ( 'NONE', #7032 ) ;
#10202 = CIRCLE ( 'NONE', #6826, 4.499999999999999112 ) ;
#10203 = DIRECTION ( 'NONE',  ( 1.000000000000000000, -0.000000000000000000, 0.000000000000000000 ) ) ;
#10204 = VECTOR ( 'NONE', #9417, 1000.000000000000000 ) ;
#10205 = CARTESIAN_POINT ( 'NONE',  ( -24.35964822603314772, 52.75208333237727487, -5.935950539335252074 ) ) ;
#10206 = LINE ( 'NONE', #6090, #10728 ) ;
#10207 = VECTOR ( 'NONE', #6622, 1000.000000000000000 ) ;
#10208 = DIRECTION ( 'NONE',  ( 1.000000000000000000, 0.000000000000000000, 0.000000000000000000 ) ) ;
#10209 = CARTESIAN_POINT ( 'NONE',  ( -25.98076211353311393, 50.72499999999985931, -2.690598923241634743 ) ) ;
#10210 = EDGE_LOOP ( 'NONE', ( #8054, #1578, #10545, #6455, #9354, #8155 ) ) ;
#10211 = ADVANCED_FACE ( 'NONE', ( #6190 ), #5736, .T. ) ;
#10212 = ORIENTED_EDGE ( 'NONE', *, *, #6691, .T. ) ;
#10213 = CARTESIAN_POINT ( 'NONE',  ( 0.000000000000000000, 0.000000000000000000, -4.974599999999998801 ) ) ;
#10215 = ORIENTED_EDGE ( 'NONE', *, *, #4312, .T. ) ;
#10214 = EDGE_CURVE ( 'NONE', #1406, #2047, #1356, .T. ) ;
#10216 = CARTESIAN_POINT ( 'NONE',  ( -27.44132740410865523, 55.89336612041927310, -4.296608737464627126 ) ) ;
#10217 = PRODUCT_CONTEXT ( 'NONE', #1170, 'mechanical' ) ;
#10218 = VECTOR ( 'NONE', #9115, 1000.000000000000000 ) ;
#10219 = ORIENTED_EDGE ( 'NONE', *, *, #2230, .T. ) ;
#10220 = CARTESIAN_POINT ( 'NONE',  ( 20.73695268571362504, 18.16262921024512167, 12.00579112326941988 ) ) ;
#10221 = CARTESIAN_POINT ( 'NONE',  ( -25.98076211353324894, 16.50000000000026290, -5.000000000000000000 ) ) ;
#10222 = CIRCLE ( 'NONE', #5959, 1.999999999999971356 ) ;
#10223 = EDGE_CURVE ( 'NONE', #6512, #2646, #1945, .T. ) ;
#10224 = CARTESIAN_POINT ( 'NONE',  ( -27.98076211353308551, 51.80416666475470322, -6.154700538379338504 ) ) ;
#10225 = CARTESIAN_POINT ( 'NONE',  ( -25.17020516978313083, 50.47708333237727629, -3.596074190997380349 ) ) ;
#10226 = CARTESIAN_POINT ( 'NONE',  ( 21.34179237787287065, 23.66094220255952152, 11.95042449705224819 ) ) ;
#10227 = FACE_OUTER_BOUND ( 'NONE', #10509, .T. ) ;
#10228 = CARTESIAN_POINT ( 'NONE',  ( -24.35964822603314417, 50.59374999904394343, -5.000000000000103029 ) ) ;
#10229 = EDGE_CURVE ( 'NONE', #1419, #3831, #4550, .T. ) ;
#10230 = VECTOR ( 'NONE', #1070, 999.9999999999998863 ) ;
#10231 = FACE_OUTER_BOUND ( 'NONE', #916, .T. ) ;
#10232 = VERTEX_POINT ( 'NONE', #10791 ) ;
#10233 = CARTESIAN_POINT ( 'NONE',  ( 2.500000000000000000, -2.357898499370432610, 3.252606517456513302E-15 ) ) ;
#10234 = ORIENTED_EDGE ( 'NONE', *, *, #9409, .F. ) ;
#10235 = CARTESIAN_POINT ( 'NONE',  ( -3.500000000000003109, 29.99999999999999645, 16.46875000000000355 ) ) ;
#10236 = ORIENTED_EDGE ( 'NONE', *, *, #2878, .F. ) ;
#10237 = CARTESIAN_POINT ( 'NONE',  ( 22.96512898726170704, 23.28924158689358848, 11.95042449705224819 ) ) ;
#10238 = FILL_AREA_STYLE ('',( #119 ) ) ;
#10239 = ADVANCED_FACE ( 'NONE', ( #1511 ), #2775, .T. ) ;
#10240 = CARTESIAN_POINT ( 'NONE',  ( 17.26579466391090634, 16.35877559204224951, 12.05147379044805866 ) ) ;
#10241 = CARTESIAN_POINT ( 'NONE',  ( 18.27511531525127353, 17.01097670698189290, 12.03680973694848966 ) ) ;
#10242 = CARTESIAN_POINT ( 'NONE',  ( -27.60187600103308014, 52.92708333237728624, -4.064049460664955760 ) ) ;
#10243 = CARTESIAN_POINT ( 'NONE',  ( -2.500000000000005773, 29.99999999999999645, 16.46875000000000355 ) ) ;
#10244 = SPHERICAL_SURFACE ( 'NONE', #7911, 3.250000000000000000 ) ;
#10245 = DIRECTION ( 'NONE',  ( 0.000000000000000000, 0.000000000000000000, -1.000000000000000000 ) ) ;
#10246 = ORIENTED_EDGE ( 'NONE', *, *, #5469, .F. ) ;
#10247 = EDGE_LOOP ( 'NONE', ( #2379, #5288, #9197, #1392, #5393, #8774 ) ) ;
#10248 = EDGE_CURVE ( 'NONE', #3903, #4955, #8618, .T. ) ;
#10249 = CARTESIAN_POINT ( 'NONE',  ( 25.98076211353311749, 56.49999999999984368, 10.00000000000000178 ) ) ;
#10250 = CARTESIAN_POINT ( 'NONE',  ( 29.49999999999999645, -3.999999999999983569, 10.00000000000000888 ) ) ;
#10251 = AXIS2_PLACEMENT_3D ( 'NONE', #4018, #5793, #4077 ) ;
#10252 = CIRCLE ( 'NONE', #3866, 1.649999999999998579 ) ;
#10253 = CARTESIAN_POINT ( 'NONE',  ( 21.25655365073496839, 18.52406763439849513, 12.00579112326941988 ) ) ;
#10254 = CARTESIAN_POINT ( 'NONE',  ( 1.035533905932743970, 27.49999999999999289, 15.60937500000000533 ) ) ;
#10255 = CARTESIAN_POINT ( 'NONE',  ( -26.79131905728310059, 52.98541666571061626, -3.596074190997381237 ) ) ;
#10256 = SURFACE_SIDE_STYLE ('',( #6863 ) ) ;
#10257 = DIRECTION ( 'NONE',  ( 1.000000000000000000, 0.000000000000000000, 0.000000000000000000 ) ) ;
#10258 = DIRECTION ( 'NONE',  ( -6.098637220230963674E-17, 1.000000000000000000, 0.000000000000000000 ) ) ;
#10259 = ORIENTED_EDGE ( 'NONE', *, *, #8341, .T. ) ;
#10260 = VECTOR ( 'NONE', #1294, 1000.000000000000000 ) ;
#10261 = CARTESIAN_POINT ( 'NONE',  ( -2.385244779468109755E-15, 32.50000000000000711, 13.65625000000000355 ) ) ;
#10262 = DIRECTION ( 'NONE',  ( 2.775557561562891351E-17, 1.000000000000000000, -8.326672684688671588E-17 ) ) ;
#10263 = CARTESIAN_POINT ( 'NONE',  ( -27.60187600103308725, 52.28541666571061342, -5.935950539335252074 ) ) ;
#10264 = CARTESIAN_POINT ( 'NONE',  ( -25.98076211353311393, 51.07499999999986784, -7.000000000000073719 ) ) ;
#10265 = STYLED_ITEM ( 'NONE', ( #3792 ), #5271 ) ;
#10266 = DIRECTION ( 'NONE',  ( 6.098637220230963674E-17, -1.000000000000000000, 0.000000000000000000 ) ) ;
#10267 = DIRECTION ( 'NONE',  ( 1.000000000000000000, 0.000000000000000000, 0.000000000000000000 ) ) ;
#10268 = ORIENTED_EDGE ( 'NONE', *, *, #9182, .T. ) ;
#10269 = EDGE_CURVE ( 'NONE', #234, #2958, #9960, .T. ) ;
#10270 = VERTEX_POINT ( 'NONE', #5687 ) ;
#10271 = DIRECTION ( 'NONE',  ( -0.000000000000000000, 0.8660254037844392627, 0.4999999999999990008 ) ) ;
#10272 = B_SPLINE_CURVE_WITH_KNOTS ( 'NONE', 3,
 ( #8333, #9106, #2290, #10630, #3171, #2389 ),
 .UNSPECIFIED., .F., .F.,
 ( 4, 2, 4 ),
 ( 0.003358874760055551890, 0.004541967308452098118, 0.005725059856848645212 ),
 .UNSPECIFIED. ) ;
#10273 = LINE ( 'NONE', #875, #7893 ) ;
#10274 = APPLICATION_PROTOCOL_DEFINITION ( 'draft international standard', 'automotive_design', 1998, #8765 ) ;
#10275 = ORIENTED_EDGE ( 'NONE', *, *, #2167, .F. ) ;
#10276 = CARTESIAN_POINT ( 'NONE',  ( 21.05771646464872404, 22.57981893131178452, 12.00579112326941988 ) ) ;
#10277 = CARTESIAN_POINT ( 'NONE',  ( 0.6920835326022565237, 4.454600218803884459, -3.597382984111579862 ) ) ;
#10278 = CARTESIAN_POINT ( 'NONE',  ( -31.74999999999995737, 0.000000000000000000, 0.000000000000000000 ) ) ;
#10279 = CARTESIAN_POINT ( 'NONE',  ( -25.17020516978313083, 52.11041666571060915, -6.403925809002825709 ) ) ;
#10280 = EDGE_CURVE ( 'NONE', #10997, #10983, #7455, .T. ) ;
#10281 = CARTESIAN_POINT ( 'NONE',  ( 24.32342464814431438, 20.41340561598360992, 11.95042449705224996 ) ) ;
#10282 = CYLINDRICAL_SURFACE ( 'NONE', #3777, 4.499999999999999112 ) ;
#10283 = B_SPLINE_CURVE_WITH_KNOTS ( 'NONE', 3,
 ( #1637, #9295, #10973, #2474 ),
 .UNSPECIFIED., .F., .F.,
 ( 4, 4 ),
 ( 2.380739282168294182E-07, 0.002044882221487568340 ),
 .UNSPECIFIED. ) ;
#10284 = EDGE_CURVE ( 'NONE', #6644, #3608, #509, .T. ) ;
#10285 = CARTESIAN_POINT ( 'NONE',  ( -27.98076211353308551, 54.02083333142136468, -3.845299461620869330 ) ) ;
#10286 = DIRECTION ( 'NONE',  ( 0.000000000000000000, 0.000000000000000000, 1.000000000000000000 ) ) ;
#10287 = VERTEX_POINT ( 'NONE', #3906 ) ;
#10288 = FACE_OUTER_BOUND ( 'NONE', #1518, .T. ) ;
#10289 = ORIENTED_EDGE ( 'NONE', *, *, #2550, .T. ) ;
#10290 = CARTESIAN_POINT ( 'NONE',  ( -1.734723475976807094E-15, 33.50000000000000000, 14.90625000000000355 ) ) ;
#10291 = ORIENTED_EDGE ( 'NONE', *, *, #1402, .F. ) ;
#10292 = CARTESIAN_POINT ( 'NONE',  ( 19.49929303312607942, 16.16195407633872350, 11.95465698723049108 ) ) ;
#10293 = FILL_AREA_STYLE_COLOUR ( '', #842 ) ;
#10294 = ADVANCED_FACE ( 'NONE', ( #556 ), #3074, .T. ) ;
#10295 = CARTESIAN_POINT ( 'NONE',  ( 19.49929303312607942, 16.16195407633872350, 11.95465698723049108 ) ) ;
#10296 = CARTESIAN_POINT ( 'NONE',  ( 22.88317621546045189, 19.71992003298075957, 12.00579112326941988 ) ) ;
#10297 = CARTESIAN_POINT ( 'NONE',  ( -25.17020516978313083, 51.00208333237728198, -3.596074190997380349 ) ) ;
#10298 = CARTESIAN_POINT ( 'NONE',  ( -2.500000000000007550, 31.03553390593274486, 16.39062500000000355 ) ) ;
#10299 = DIRECTION ( 'NONE',  ( 0.000000000000000000, 0.000000000000000000, 1.000000000000000000 ) ) ;
#10300 = CARTESIAN_POINT ( 'NONE',  ( 21.21106610644839208, 53.49999999999983658, 14.50000000000000000 ) ) ;
#10301 = EDGE_CURVE ( 'NONE', #3429, #234, #6560, .T. ) ;
#10302 = VERTEX_POINT ( 'NONE', #4913 ) ;
#10303 = ADVANCED_FACE ( 'NONE', ( #9021 ), #1410, .F. ) ;
#10304 = EDGE_LOOP ( 'NONE', ( #8223, #8321, #2133 ) ) ;
#10305 = CARTESIAN_POINT ( 'NONE',  ( 19.05040816462259556, 17.06282649731835122, 12.00984920396035172 ) ) ;
#10306 = CARTESIAN_POINT ( 'NONE',  ( 2.000000000000000000, -1.329782007511007169, -0.7677499999999988223 ) ) ;
#10307 = CARTESIAN_POINT ( 'NONE',  ( 19.69775075566884226, 17.43975236193677603, 12.00579112326941988 ) ) ;
#10308 = CARTESIAN_POINT ( 'NONE',  ( 1.767766952966377314, 28.23223304703363112, 14.43750000000000178 ) ) ;
#10309 = CARTESIAN_POINT ( 'NONE',  ( 2.756197834950227410, 3.027510591568626896, -3.223146290109805356 ) ) ;
#10310 = CARTESIAN_POINT ( 'NONE',  ( -26.79131905728310059, 54.85208333237729050, -6.403925809002825709 ) ) ;
#10311 = DIRECTION ( 'NONE',  ( 0.6587175828649982634, -0.7523902883640206651, 3.989863994746656317E-16 ) ) ;
#10312 = CARTESIAN_POINT ( 'NONE',  ( -25.18193375740463935, 57.38490676151830172, -3.163901733045028752 ) ) ;
#10313 = CARTESIAN_POINT ( 'NONE',  ( 2.000000000000000000, 0.000000000000000000, 0.000000000000000000 ) ) ;
#10314 = ORIENTED_EDGE ( 'NONE', *, *, #3211, .T. ) ;
#10315 = CYLINDRICAL_SURFACE ( 'NONE', #1035, 2.100000000000000089 ) ;
#10316 = AXIS2_PLACEMENT_3D ( 'NONE', #2530, #5862, #8302 ) ;
#10317 = CARTESIAN_POINT ( 'NONE',  ( 4.553649124439118623E-15, 27.49999999999999289, 15.53125000000000355 ) ) ;
#10318 = CARTESIAN_POINT ( 'NONE',  ( -2.500000000000007550, 31.03553390593274486, 15.14062500000000355 ) ) ;
#10319 = EDGE_CURVE ( 'NONE', #3414, #783, #4071, .T. ) ;
#10320 = CARTESIAN_POINT ( 'NONE',  ( -24.35964822603314772, 54.85208333237728340, -5.935950539335252074 ) ) ;
#10321 = LINE ( 'NONE', #3377, #8780 ) ;
#10322 = VECTOR ( 'NONE', #3296, 1000.000000000000000 ) ;
#10323 = DIRECTION ( 'NONE',  ( 1.000000000000000000, 0.000000000000000000, 0.000000000000000000 ) ) ;
#10324 = DIRECTION ( 'NONE',  ( -0.7055570967602625698, 0.7055570967602456944, 0.06616922564518108729 ) ) ;
#10325 = EDGE_LOOP ( 'NONE', ( #2506, #2009, #5014, #9697 ) ) ;
#10326 = VERTEX_POINT ( 'NONE', #3234 ) ;
#10327 = CARTESIAN_POINT ( 'NONE',  ( -26.51666049839534622, 54.89373926088290290, -3.000000000000131006 ) ) ;
#10328 = CARTESIAN_POINT ( 'NONE',  ( 29.49999999999999645, -3.999999999999983569, 10.00000000000000888 ) ) ;
#10329 = CARTESIAN_POINT ( 'NONE',  ( -3.061616997868384127E-16, 30.00000000000000000, -7.500000000000003553 ) ) ;
#10330 = VERTEX_POINT ( 'NONE', #8181 ) ;
#10331 = CARTESIAN_POINT ( 'NONE',  ( 2.000000000000000000, 1.773042676681340524, -2.059984127722458425E-15 ) ) ;
#10332 = CYLINDRICAL_SURFACE ( 'NONE', #8609, 2.500000000000000888 ) ;
#10333 = VECTOR ( 'NONE', #1531, 1000.000000000000000 ) ;
#10334 = CARTESIAN_POINT ( 'NONE',  ( 22.98142095123195716, 18.50759888342988546, 11.95042449705211141 ) ) ;
#10335 = FACE_OUTER_BOUND ( 'NONE', #10381, .T. ) ;
#10336 = CARTESIAN_POINT ( 'NONE',  ( -25.98076211353311393, 51.46874999904394343, -6.871901078670400231 ) ) ;
#10337 = CARTESIAN_POINT ( 'NONE',  ( 2.500000000000000888, 3.061616997868384127E-16, -4.974599999999998801 ) ) ;
#10338 = ORIENTED_EDGE ( 'NONE', *, *, #3531, .T. ) ;
#10339 = CARTESIAN_POINT ( 'NONE',  ( 29.49999999999999645, 2.000000000000001776, -10.50000000000000355 ) ) ;
#10340 = PRODUCT ( 'Tension Return Spring', 'Tension Return Spring', '', ( #10217 ) ) ;
#10341 = ORIENTED_EDGE ( 'NONE', *, *, #500, .T. ) ;
#10342 = CARTESIAN_POINT ( 'NONE',  ( -3.500000000000002665, 29.72450764647708255, 16.48359592357600434 ) ) ;
#10343 = ORIENTED_EDGE ( 'NONE', *, *, #8787, .F. ) ;
#10344 = CARTESIAN_POINT ( 'NONE',  ( 17.39179625728592882, 16.28601130006924791, 12.04260150961189524 ) ) ;
#10345 = EDGE_CURVE ( 'NONE', #7434, #1907, #9137, .T. ) ;
#10346 = DIRECTION ( 'NONE',  ( 0.000000000000000000, 0.000000000000000000, -1.000000000000000000 ) ) ;
#10347 = CARTESIAN_POINT ( 'NONE',  ( 22.98009469009668138, 21.94211999725310491, 12.00579112326941988 ) ) ;
#10348 = CARTESIAN_POINT ( 'NONE',  ( -26.79131905728310059, 49.95208333237728482, -6.403925809002825709 ) ) ;
#10349 = CARTESIAN_POINT ( 'NONE',  ( -1.035533905932742638, 32.50000000000000000, 13.73437500000000533 ) ) ;
#10350 = CARTESIAN_POINT ( 'NONE',  ( -21.21106610644865498, 13.49999999999941913, -9.500000000000000000 ) ) ;
#10351 = CARTESIAN_POINT ( 'NONE',  ( -26.92841756856055824, 58.32602275755382948, -6.761469286193118933 ) ) ;
#10352 = ORIENTED_EDGE ( 'NONE', *, *, #4025, .F. ) ;
#10353 = ADVANCED_FACE ( 'NONE', ( #1569 ), #4969, .F. ) ;
#10354 = ORIENTED_EDGE ( 'NONE', *, *, #10658, .T. ) ;
#10355 = EDGE_CURVE ( 'NONE', #4005, #3988, #6732, .T. ) ;
#10356 = DIRECTION ( 'NONE',  ( -0.000000000000000000, -0.000000000000000000, -1.000000000000000000 ) ) ;
#10357 = DIRECTION ( 'NONE',  ( 0.000000000000000000, 0.000000000000000000, 1.000000000000000000 ) ) ;
#10358 =( BOUNDED_CURVE ( )  B_SPLINE_CURVE ( 2, ( #5084, #4075, #3298, #8346, #5851, #9964, #6736, #9233, #5028 ),
 .UNSPECIFIED., .F., .F. ) 
 B_SPLINE_CURVE_WITH_KNOTS ( ( 3, 2, 2, 2, 3 ),
 ( 0.1944444444444444198, 0.2037037037037036924, 0.2222222222222222099, 0.2407407407407407274, 0.2500000000000000000 ),
 .UNSPECIFIED. ) 
 CURVE ( )  GEOMETRIC_REPRESENTATION_ITEM ( )  RATIONAL_B_SPLINE_CURVE ( ( 0.9330127018922192983, 0.9330127018922191873, 1.000000000000000000, 0.8660254037844387076, 1.000000000000000000, 0.8660254037844387076, 1.000000000000000000, 0.9330127018922191873, 0.9330127018922192983 ) ) 
 REPRESENTATION_ITEM ( '' )  );
#10359 = DIRECTION ( 'NONE',  ( 1.000000000000000000, 6.098637220230964906E-17, 6.308085367188384325E-16 ) ) ;
#10360 = FACE_OUTER_BOUND ( 'NONE', #3446, .T. ) ;
#10361 = DIRECTION ( 'NONE',  ( 0.5150380749100549327, 1.049727191138617956E-16, 0.8571673007021118895 ) ) ;
#10362 = CARTESIAN_POINT ( 'NONE',  ( -27.60187600103308370, 52.16874999904395338, -5.000000000000103029 ) ) ;
#10363 = FACE_OUTER_BOUND ( 'NONE', #3551, .T. ) ;
#10364 = DIRECTION ( 'NONE',  ( 0.000000000000000000, 1.000000000000000000, -1.224646799147353207E-16 ) ) ;
#10365 = AXIS2_PLACEMENT_3D ( 'NONE', #7152, #5499, #5382 ) ;
#10366 = ORIENTED_EDGE ( 'NONE', *, *, #6021, .T. ) ;
#10367 = SURFACE_STYLE_USAGE ( .BOTH. , #8647 ) ;
#10368 = CARTESIAN_POINT ( 'NONE',  ( 2.500000000000008438, 30.00000000000000711, 15.84375000000000355 ) ) ;
#10369 = CARTESIAN_POINT ( 'NONE',  ( -2.385244779468109755E-15, 32.50000000000000711, 16.15625000000000355 ) ) ;
#10370 = CARTESIAN_POINT ( 'NONE',  ( -25.98076211353311749, 56.99999999999884182, -7.000000000000094147 ) ) ;
#10371 = CARTESIAN_POINT ( 'NONE',  ( -25.44486372867087809, 55.24373926088289721, -7.000000000000075495 ) ) ;
#10372 = CARTESIAN_POINT ( 'NONE',  ( -1.219727444046192735E-16, 2.000000000000000000, 15.49999999999999645 ) ) ;
#10373 = LINE ( 'NONE', #4389, #1625 ) ;
#10374 = CIRCLE ( 'NONE', #7007, 0.1199999999999998845 ) ;
#10375 = ORIENTED_EDGE ( 'NONE', *, *, #8639, .F. ) ;
#10376 = VECTOR ( 'NONE', #1764, 1000.000000000000000 ) ;
#10377 = ORIENTED_EDGE ( 'NONE', *, *, #293, .T. ) ;
#10378 = FACE_OUTER_BOUND ( 'NONE', #10055, .T. ) ;
#10379 = DIRECTION ( 'NONE',  ( -1.000000000000000000, -0.000000000000000000, -0.000000000000000000 ) ) ;
#10380 = APPLICATION_PROTOCOL_DEFINITION ( 'draft international standard', 'automotive_design', 1998, #10047 ) ;
#10381 = EDGE_LOOP ( 'NONE', ( #6213, #7404, #639, #10399 ) ) ;
#10382 = EDGE_CURVE ( 'NONE', #5854, #6011, #1741, .T. ) ;
#10383 = CARTESIAN_POINT ( 'NONE',  ( 3.200000000000000178, 3.031088913245510774, -1.750000000000042411 ) ) ;
#10384 = AXIS2_PLACEMENT_3D ( 'NONE', #659, #8329, #2447 ) ;
#10385 = FACE_OUTER_BOUND ( 'NONE', #7849, .T. ) ;
#10386 = CIRCLE ( 'NONE', #3284, 2.649999999999991029 ) ;
#10387 = CIRCLE ( 'NONE', #8077, 1.649999999999989919 ) ;
#10388 = VECTOR ( 'NONE', #6487, 1000.000000000000000 ) ;
#10389 = CARTESIAN_POINT ( 'NONE',  ( 24.03139851132786831, 19.63770821034670533, 11.95042449705224996 ) ) ;
#10390 = DIRECTION ( 'NONE',  ( 1.000000000000000000, 0.000000000000000000, -0.000000000000000000 ) ) ;
#10391 = CARTESIAN_POINT ( 'NONE',  ( -25.17020516978313083, 51.41041666571061342, -6.403925809002825709 ) ) ;
#10392 = CIRCLE ( 'NONE', #91, 0.2500000000000002220 ) ;
#10393 = CARTESIAN_POINT ( 'NONE',  ( 25.49999999999999645, -3.999999999999986233, -4.999999999999992006 ) ) ;
#10394 = ORIENTED_EDGE ( 'NONE', *, *, #8923, .T. ) ;
#10395 = DIRECTION ( 'NONE',  ( 1.000000000000000000, -0.000000000000000000, -0.000000000000000000 ) ) ;
#10396 = EDGE_LOOP ( 'NONE', ( #2584, #10291, #5030, #10830 ) ) ;
#10397 = CARTESIAN_POINT ( 'NONE',  ( 0.9693646802875628410, 32.52740819067395961, 12.58031658473306713 ) ) ;
#10398 = VECTOR ( 'NONE', #8881, 1000.000000000000000 ) ;
#10399 = ORIENTED_EDGE ( 'NONE', *, *, #8723, .F. ) ;
#10400 = CARTESIAN_POINT ( 'NONE',  ( 16.19085831639751305, 17.34467558953444311, 12.14735994959144350 ) ) ;
#10401 = DIRECTION ( 'NONE',  ( 0.000000000000000000, 0.000000000000000000, 1.000000000000000000 ) ) ;
#10402 = CARTESIAN_POINT ( 'NONE',  ( 20.47715220320264962, 17.98190999816754498, 12.00579112326941988 ) ) ;
#10403 = B_SPLINE_CURVE_WITH_KNOTS ( 'NONE', 3,
 ( #1998, #5446, #4779, #6216, #8834 ),
 .UNSPECIFIED., .F., .F.,
 ( 4, 1, 4 ),
 ( 0.000000000000000000, 0.002309401076758505356, 0.004618802153517010713 ),
 .UNSPECIFIED. ) ;
#10405 = CARTESIAN_POINT ( 'NONE',  ( -24.35964822603314417, 51.11874999904394912, -5.000000000000103029 ) ) ;
#10404 = AXIS2_PLACEMENT_3D ( 'NONE', #10130, #4918, #6564 ) ;
#10406 = DIRECTION ( 'NONE',  ( -0.000000000000000000, -1.000000000000000000, -0.000000000000000000 ) ) ;
#10407 = PLANE ( 'NONE',  #2767 ) ;
#10408 = FACE_OUTER_BOUND ( 'NONE', #8731, .T. ) ;
#10409 = APPLICATION_CONTEXT ( 'automotive_design' ) ;
#10410 = EDGE_CURVE ( 'NONE', #7320, #3058, #4902, .T. ) ;
#10411 = EDGE_LOOP ( 'NONE', ( #3157, #5170, #67, #2749 ) ) ;
#10412 = ORIENTED_EDGE ( 'NONE', *, *, #8339, .T. ) ;
#10413 = CYLINDRICAL_SURFACE ( 'NONE', #10043, 1.999999999999971356 ) ;
#10415 = DIRECTION ( 'NONE',  ( -0.000000000000000000, -0.000000000000000000, 1.000000000000000000 ) ) ;
#10414 = AXIS2_PLACEMENT_3D ( 'NONE', #2977, #6351, #395 ) ;
#10416 = SURFACE_STYLE_USAGE ( .BOTH. , #4482 ) ;
#10417 = CARTESIAN_POINT ( 'NONE',  ( -26.98076211353408382, 57.99999999999985789, -3.267949192431818251 ) ) ;
#10418 = AXIS2_PLACEMENT_3D ( 'NONE', #5279, #3556, #6157 ) ;
#10419 = DIRECTION ( 'NONE',  ( 0.000000000000000000, 0.000000000000000000, 1.000000000000000000 ) ) ;
#10420 = CARTESIAN_POINT ( 'NONE',  ( 4.211140560182196957, -2.431303136016555122, -3.745885042887436622 ) ) ;
#10421 = EDGE_CURVE ( 'NONE', #8739, #10063, #626, .T. ) ;
#10422 = FACE_OUTER_BOUND ( 'NONE', #9223, .T. ) ;
#10423 = CARTESIAN_POINT ( 'NONE',  ( 1.449747468305833120, 33.50000000000000000, 14.82812500000000178 ) ) ;
#10424 = CARTESIAN_POINT ( 'NONE',  ( -26.98076211353408382, 57.99999999999985789, -3.267949192431818251 ) ) ;
#10425 = VERTEX_POINT ( 'NONE', #4121 ) ;
#10426 = ADVANCED_FACE ( 'NONE', ( #5138 ), #1522, .T. ) ;
#10427 = CARTESIAN_POINT ( 'NONE',  ( -1.720978244806810498, 31.81455566112594013, 14.81030841526694175 ) ) ;
#10428 =( BOUNDED_CURVE ( )  B_SPLINE_CURVE ( 2, ( #2075, #7176, #6233, #1121, #8854 ),
 .UNSPECIFIED., .F., .F. ) 
 B_SPLINE_CURVE_WITH_KNOTS ( ( 3, 2, 3 ),
 ( 0.000000000000000000, 0.01851851851851851749, 0.02777777777777777971 ),
 .UNSPECIFIED. ) 
 CURVE ( )  GEOMETRIC_REPRESENTATION_ITEM ( )  RATIONAL_B_SPLINE_CURVE ( ( 1.000000000000000000, 0.8660254037844387076, 1.000000000000000000, 0.9330127018922192983, 0.9330127018922194093 ) ) 
 REPRESENTATION_ITEM ( '' )  );
#10429 = AXIS2_PLACEMENT_3D ( 'NONE', #3412, #4424, #5144 ) ;
#10430 = AXIS2_PLACEMENT_3D ( 'NONE', #6958, #9674, #2069 ) ;
#10431 = CARTESIAN_POINT ( 'NONE',  ( -2.469212770973128190, 29.60886282244813117, 16.49922112211940117 ) ) ;
#10432 = UNCERTAINTY_MEASURE_WITH_UNIT (LENGTH_MEASURE( 1.000000000000000082E-05 ), #7554, 'distance_accuracy_value', 'NONE');
#10433 = DIRECTION ( 'NONE',  ( 0.000000000000000000, 0.000000000000000000, -1.000000000000000000 ) ) ;
#10434 = DIRECTION ( 'NONE',  ( 0.000000000000000000, 0.000000000000000000, 1.000000000000000000 ) ) ;
#10435 = EDGE_CURVE ( 'NONE', #4729, #2494, #8258, .T. ) ;
#10436 = PRODUCT_DEFINITION_SHAPE ( 'NONE', 'NONE',  #11010 ) ;
#10437 = DIRECTION ( 'NONE',  ( -1.000000000000000000, -0.000000000000000000, -0.000000000000000000 ) ) ;
#10438 = VECTOR ( 'NONE', #3282, 1000.000000000000114 ) ;
#10439 = DIRECTION ( 'NONE',  ( 0.000000000000000000, 0.000000000000000000, -1.000000000000000000 ) ) ;
#10440 = VERTEX_POINT ( 'NONE', #4244 ) ;
#10441 = EDGE_LOOP ( 'NONE', ( #770, #1241, #10659, #1192, #1306, #2471 ) ) ;
#10442 = DIRECTION ( 'NONE',  ( 0.000000000000000000, 0.000000000000000000, 1.000000000000000000 ) ) ;
#10443 = EDGE_CURVE ( 'NONE', #2547, #2239, #9196, .T. ) ;
#10444 = CARTESIAN_POINT ( 'NONE',  ( 2.059999999999998721, 0.000000000000000000, -0.3080913168122742518 ) ) ;
#10445 = APPLICATION_PROTOCOL_DEFINITION ( 'draft international standard', 'automotive_design', 1998, #10820 ) ;
#10446 = ORIENTED_EDGE ( 'NONE', *, *, #3221, .T. ) ;
#10447 = CIRCLE ( 'NONE', #10617, 24.99999999999999645 ) ;
#10448 = DIRECTION ( 'NONE',  ( 0.000000000000000000, -1.000000000000000000, 1.287488025362403787E-15 ) ) ;
#10449 = CARTESIAN_POINT ( 'NONE',  ( 0.3126073911696448659, -4.041451884327390331, 2.328673539876467720E-14 ) ) ;
#10450 = VECTOR ( 'NONE', #9528, 1000.000000000000000 ) ;
#10451 = CARTESIAN_POINT ( 'NONE',  ( 22.99824548812224378, 19.95783898428147651, 11.00732503135576401 ) ) ;
#10452 = EDGE_CURVE ( 'NONE', #2599, #9431, #2976, .T. ) ;
#10453 = FACE_OUTER_BOUND ( 'NONE', #4782, .T. ) ;
#10454 = CARTESIAN_POINT ( 'NONE',  ( -25.17020516978313083, 52.57708333237728482, -3.596074190997380349 ) ) ;
#10455 = CARTESIAN_POINT ( 'NONE',  ( 27.50000000000001066, -8.499999999999982236, 10.00000000000001243 ) ) ;
#10456 = VERTEX_POINT ( 'NONE', #1171 ) ;
#10457 = CARTESIAN_POINT ( 'NONE',  ( 34.99999999999987210, -3.999999999999989786, -7.149999999999991473 ) ) ;
#10458 = EDGE_LOOP ( 'NONE', ( #2032, #6793, #756, #8599 ) ) ;
#10459 = CARTESIAN_POINT ( 'NONE',  ( -1.814555661125939912, 31.72097824480680117, 12.81469158473306713 ) ) ;
#10460 = ORIENTED_EDGE ( 'NONE', *, *, #6280, .F. ) ;
#10461 = CARTESIAN_POINT ( 'NONE',  ( 23.79237391907785693, 22.55645663433636017, 11.95042449705224819 ) ) ;
#10462 =( NAMED_UNIT ( * ) SI_UNIT ( $, .STERADIAN. ) SOLID_ANGLE_UNIT ( ) );
#10463 = CARTESIAN_POINT ( 'NONE',  ( 0.1999999999999987899, 0.000000000000000000, 0.000000000000000000 ) ) ;
#10464 = CARTESIAN_POINT ( 'NONE',  ( 16.47160909572790999, 17.06392481020577279, 13.12322671172946897 ) ) ;
#10465 = CARTESIAN_POINT ( 'NONE',  ( -25.17020516978313083, 55.20208333237728482, -3.596074190997380349 ) ) ;
#10466 = FILL_AREA_STYLE ('',( #10518 ) ) ;
#10467 = CARTESIAN_POINT ( 'NONE',  ( 29.49999999999999289, 2.000000000000001776, 15.49999999999999822 ) ) ;
#10468 = DIRECTION ( 'NONE',  ( 0.000000000000000000, 0.000000000000000000, 1.000000000000000000 ) ) ;
#10469 = ORIENTED_EDGE ( 'NONE', *, *, #10803, .F. ) ;
#10470 = CARTESIAN_POINT ( 'NONE',  ( 2.000000000000000000, 1.773042676681340524, -2.059984127722458425E-15 ) ) ;
#10471 = CARTESIAN_POINT ( 'NONE',  ( 0.000000000000000000, 0.000000000000000000, 2.500000000000000000 ) ) ;
#10472 = FILL_AREA_STYLE_COLOUR ( '', #3975 ) ;
#10473 = ADVANCED_FACE ( 'NONE', ( #2909 ), #3789, .F. ) ;
#10474 = CARTESIAN_POINT ( 'NONE',  ( 0.000000000000000000, 0.000000000000000000, 0.000000000000000000 ) ) ;
#10475 = DIRECTION ( 'NONE',  ( -1.000000000000000000, 0.000000000000000000, 0.000000000000000000 ) ) ;
#10476 = LINE ( 'NONE', #7188, #2806 ) ;
#10477 = APPLICATION_CONTEXT ( 'automotive_design' ) ;
#10478 = SURFACE_STYLE_USAGE ( .BOTH. , #243 ) ;
#10479 = CARTESIAN_POINT ( 'NONE',  ( -2.474873734152916338, 27.52512626584707789, 14.12500000000000355 ) ) ;
#10480 = CARTESIAN_POINT ( 'NONE',  ( -26.25045812061784289, 0.000000000000000000, -5.000000000000000000 ) ) ;
#10481 = VERTEX_POINT ( 'NONE', #7013 ) ;
#10482 = FACE_OUTER_BOUND ( 'NONE', #7246, .T. ) ;
#10483 = CARTESIAN_POINT ( 'NONE',  ( 0.9693646802875698354, 27.47259180932603684, 15.35718341526694530 ) ) ;
#10484 = CARTESIAN_POINT ( 'NONE',  ( -1.035533905932736420, 27.49999999999998934, 14.20312500000000355 ) ) ;
#10485 = CARTESIAN_POINT ( 'NONE',  ( 19.77604874367146692, 21.01153129092389094, 12.00579112326941988 ) ) ;
#10486 = EDGE_CURVE ( 'NONE', #1437, #6429, #6699, .T. ) ;
#10487 = CARTESIAN_POINT ( 'NONE',  ( 29.50000000000000711, 1.799097979968134709E-15, -2.500000000000000000 ) ) ;
#10488 = CARTESIAN_POINT ( 'NONE',  ( -23.98076211353314235, 53.05833333333319501, -6.154700538379337615 ) ) ;
#10489 = EDGE_CURVE ( 'NONE', #10302, #3381, #8835, .T. ) ;
#10490 = CARTESIAN_POINT ( 'NONE',  ( -26.98076211353309972, 51.36666666666653214, -3.267949192431252037 ) ) ;
#10491 = CARTESIAN_POINT ( 'NONE',  ( -26.79131905728310059, 54.32708333237727771, -6.403925809002825709 ) ) ;
#10492 = B_SPLINE_CURVE_WITH_KNOTS ( 'NONE', 3,
 ( #6032, #6750, #2533, #5208, #5918, #10312, #2708, #6083, #9472, #8644 ),
 .UNSPECIFIED., .F., .F.,
 ( 4, 2, 2, 2, 4 ),
 ( 6.952433221959954168E-18, 0.0003978633013915846856, 0.0007957266027831624323, 0.001193589904174740179, 0.001591453205566317926 ),
 .UNSPECIFIED. ) ;
#10493 = CARTESIAN_POINT ( 'NONE',  ( 29.49999999999999645, -3.999999999999986233, -4.999999999999991118 ) ) ;
#10494 = CARTESIAN_POINT ( 'NONE',  ( -23.98076211353314235, 55.15833333333319644, -6.154700538379337615 ) ) ;
#10495 = VERTEX_POINT ( 'NONE', #3680 ) ;
#10496 = VERTEX_POINT ( 'NONE', #6278 ) ;
#10497 = CARTESIAN_POINT ( 'NONE',  ( -25.98076211353311393, 50.63749999808803892, -3.000000000000132339 ) ) ;
#10498 = EDGE_CURVE ( 'NONE', #10159, #5796, #10252, .T. ) ;
#10499 = CARTESIAN_POINT ( 'NONE',  ( 34.99999999999999289, -9.999999999999998224, 15.50000000000001243 ) ) ;
#10500 = ITEM_DEFINED_TRANSFORMATION ( 'NONE', 'NONE', #298,  #308 ) ;
#10501 = EDGE_LOOP ( 'NONE', ( #6781, #8052, #8727, #3049 ) ) ;
#10502 = EDGE_CURVE ( 'NONE', #10839, #1493, #2800, .T. ) ;
#10503 = CARTESIAN_POINT ( 'NONE',  ( 2.000000000000000000, 1.773042676681340524, -2.059984127722458425E-15 ) ) ;
#10504 = VECTOR ( 'NONE', #2244, 1000.000000000000000 ) ;
#10505 = CARTESIAN_POINT ( 'NONE',  ( -24.35964822603314772, 50.36041666571061626, -4.064049460664953983 ) ) ;
#10506 = CARTESIAN_POINT ( 'NONE',  ( 20.78941077755876776, 23.50360388977173187, 10.95195840513859231 ) ) ;
#10507 = ORIENTED_EDGE ( 'NONE', *, *, #8990, .T. ) ;
#10508 = CARTESIAN_POINT ( 'NONE',  ( -25.17020516978313083, 54.21041666571061057, -6.403925809002825709 ) ) ;
#10509 = EDGE_LOOP ( 'NONE', ( #8711, #715, #10559, #1279 ) ) ;
#10510 = DIRECTION ( 'NONE',  ( -0.000000000000000000, -0.000000000000000000, -1.000000000000000000 ) ) ;
#10511 = ORIENTED_EDGE ( 'NONE', *, *, #1354, .F. ) ;
#10512 = CARTESIAN_POINT ( 'NONE',  ( 2.500000000000008438, 30.00000000000000711, 14.59375000000000178 ) ) ;
#10513 = ORIENTED_EDGE ( 'NONE', *, *, #6516, .F. ) ;
#10514 = CARTESIAN_POINT ( 'NONE',  ( 23.84774077504003031, 19.42364242282459230, 10.95195840513859231 ) ) ;
#10515 = CARTESIAN_POINT ( 'NONE',  ( 20.77365933115271446, 23.55783661745384094, 11.95042449705224819 ) ) ;
#10516 = CARTESIAN_POINT ( 'NONE',  ( 17.17871587691444546, 17.77103159139232957, 13.12322671172946897 ) ) ;
#10517 = CARTESIAN_POINT ( 'NONE',  ( -27.44132332588852918, 55.71836679495081057, -4.296600269257925930 ) ) ;
#10518 = FILL_AREA_STYLE_COLOUR ( '', #9184 ) ;
#10519 = CIRCLE ( 'NONE', #5372, 3.500000000000000000 ) ;
#10520 = CARTESIAN_POINT ( 'NONE',  ( -3.355112389629170799, 2.681727112203152963, -0.2256878752776689534 ) ) ;
#10521 = CARTESIAN_POINT ( 'NONE',  ( 0.000000000000000000, 0.000000000000000000, 0.000000000000000000 ) ) ;
#10522 = ORIENTED_EDGE ( 'NONE', *, *, #2687, .T. ) ;
#10523 = EDGE_LOOP ( 'NONE', ( #9741, #1057, #3794, #3963 ) ) ;
#10524 = CARTESIAN_POINT ( 'NONE',  ( 25.58039891549807976, 2.000000000000002665, -2.500000000000000000 ) ) ;
#10525 = CARTESIAN_POINT ( 'NONE',  ( 3.078243469714878167, 3.710888496608943488, 0.5725525826504455074 ) ) ;
#10526 = CARTESIAN_POINT ( 'NONE',  ( 24.49999999999999289, -3.999999999999983569, 10.00000000000000888 ) ) ;
#10527 = DIRECTION ( 'NONE',  ( 0.000000000000000000, 0.000000000000000000, -1.000000000000000000 ) ) ;
#10528 = CARTESIAN_POINT ( 'NONE',  ( 29.49999999999999645, 2.000000000000001776, -5.500000000000000000 ) ) ;
#10529 = CARTESIAN_POINT ( 'NONE',  ( -27.44132740410865523, 55.89336612041927310, -4.296608737464627126 ) ) ;
#10530 = CARTESIAN_POINT ( 'NONE',  ( -27.60187600103308014, 55.69181177618367684, -4.629976867109323990 ) ) ;
#10531 = DIRECTION ( 'NONE',  ( -1.000000000000000000, 0.000000000000000000, 0.000000000000000000 ) ) ;
#10532 = CARTESIAN_POINT ( 'NONE',  ( 1.383578242660662871, 26.47259180932604039, 16.60718341526694175 ) ) ;
#10533 = CYLINDRICAL_SURFACE ( 'NONE', #8441, 1.999999999999971356 ) ;
#10534 = ORIENTED_EDGE ( 'NONE', *, *, #10435, .F. ) ;
#10535 = DIRECTION ( 'NONE',  ( 6.098637220230963674E-17, -1.000000000000000000, 0.000000000000000000 ) ) ;
#10536 = CARTESIAN_POINT ( 'NONE',  ( -2.500000000000004885, 29.80321974748363090, 16.48359592357600434 ) ) ;
#10537 = CARTESIAN_POINT ( 'NONE',  ( 2.500000000000008438, 30.00000000000000711, 15.84375000000000355 ) ) ;
#10538 = CARTESIAN_POINT ( 'NONE',  ( 20.23853826540680600, 19.71164639310234534, 12.00579112326941988 ) ) ;
#10539 = CARTESIAN_POINT ( 'NONE',  ( 0.02539999999999975264, 0.000000000000000000, 0.000000000000000000 ) ) ;
#10540 = DIRECTION ( 'NONE',  ( 0.000000000000000000, 0.000000000000000000, -1.000000000000000000 ) ) ;
#10541 = CARTESIAN_POINT ( 'NONE',  ( -3.436319922987618902, 2.634841920961291439, -3.531542292955721862 ) ) ;
#10542 = CARTESIAN_POINT ( 'NONE',  ( -27.60187600103308370, 52.34374999904394343, -5.000000000000103029 ) ) ;
#10543 = CARTESIAN_POINT ( 'NONE',  ( 4.000000000000003553, 0.000000000000000000, 0.000000000000000000 ) ) ;
#10544 = CARTESIAN_POINT ( 'NONE',  ( -27.98076211353308551, 55.39166666666653072, -6.154700538379338504 ) ) ;
#10545 = ORIENTED_EDGE ( 'NONE', *, *, #9398, .F. ) ;
#10546 = CARTESIAN_POINT ( 'NONE',  ( -26.51666049839535688, 54.60626073911682710, -7.000000000000071942 ) ) ;
#10547 = DIRECTION ( 'NONE',  ( 1.248995262339999580E-16, -0.7071067811865463515, -0.7071067811865487940 ) ) ;
#10548 = ORIENTED_EDGE ( 'NONE', *, *, #2819, .F. ) ;
#10549 = AXIS2_PLACEMENT_3D ( 'NONE', #2375, #8268, #651 ) ;
#10550 = LINE ( 'NONE', #9599, #1877 ) ;
#10551 = DIRECTION ( 'NONE',  ( 0.000000000000000000, 0.000000000000000000, -1.000000000000000000 ) ) ;
#10552 = VECTOR ( 'NONE', #10359, 1000.000000000000000 ) ;
#10553 = CARTESIAN_POINT ( 'NONE',  ( 19.32262643072814967, 17.24627075153934541, 11.00732576902737492 ) ) ;
#10554 = EDGE_CURVE ( 'NONE', #8937, #7325, #5811, .T. ) ;
#10555 = AXIS2_PLACEMENT_3D ( 'NONE', #7886, #3607, #368 ) ;
#10556 = ORIENTED_EDGE ( 'NONE', *, *, #9478, .F. ) ;
#10557 = EDGE_CURVE ( 'NONE', #9304, #10287, #1019, .T. ) ;
#10558 = CARTESIAN_POINT ( 'NONE',  ( -24.35964822603314417, 54.79374999904394627, -5.000000000000103029 ) ) ;
#10559 = ORIENTED_EDGE ( 'NONE', *, *, #7769, .T. ) ;
#10560 = DIRECTION ( 'NONE',  ( 1.000000000000000000, 6.098637220230963674E-17, 1.156482317317871478E-16 ) ) ;
#10561 = VERTEX_POINT ( 'NONE', #8014 ) ;
#10562 = CARTESIAN_POINT ( 'NONE',  ( -2.472591809326046608, 28.89829686842208289, 14.29906658473306358 ) ) ;
#10563 = VECTOR ( 'NONE', #3870, 1000.000000000000000 ) ;
#10564 = VERTEX_POINT ( 'NONE', #4417 ) ;
#10565 = AXIS2_PLACEMENT_3D ( 'NONE', #10186, #2644, #6963 ) ;
#10566 = CARTESIAN_POINT ( 'NONE',  ( 18.86745781575159242, 21.66267592685425569, 11.95042449705185561 ) ) ;
#10567 = AXIS2_PLACEMENT_3D ( 'NONE', #1721, #3881, #2947 ) ;
#10568 = CARTESIAN_POINT ( 'NONE',  ( 19.12295744889739879, 19.47009535162641569, 11.95042449705107224 ) ) ;
#10569 = CARTESIAN_POINT ( 'NONE',  ( 19.32345233471135515, 17.12110500680467240, 13.00476395487764947 ) ) ;
#10570 = EDGE_CURVE ( 'NONE', #4079, #3725, #1197, .T. ) ;
#10571 = CIRCLE ( 'NONE', #9679, 4.500000000000000000 ) ;
#10572 = DIRECTION ( 'NONE',  ( -1.000000000000000000, -0.000000000000000000, -0.000000000000000000 ) ) ;
#10573 = CIRCLE ( 'NONE', #2235, 0.2000000000000000944 ) ;
#10574 = FACE_OUTER_BOUND ( 'NONE', #8020, .T. ) ;
#10575 = FACE_OUTER_BOUND ( 'NONE', #10632, .T. ) ;
#10576 = ORIENTED_EDGE ( 'NONE', *, *, #3580, .F. ) ;
#10577 = ORIENTED_EDGE ( 'NONE', *, *, #498, .F. ) ;
#10578 = EDGE_CURVE ( 'NONE', #2294, #281, #8849, .T. ) ;
#10579 = CARTESIAN_POINT ( 'NONE',  ( 22.88317621546045189, 19.71992003298075957, 12.00579112326941988 ) ) ;
#10580 = DIRECTION ( 'NONE',  ( -1.000000000000000000, 9.251858538542971828E-16, 0.000000000000000000 ) ) ;
#10581 = CYLINDRICAL_SURFACE ( 'NONE', #9484, 4.499999999999999112 ) ;
#10582 = CIRCLE ( 'NONE', #7374, 4.250000000000000000 ) ;
#10583 = CARTESIAN_POINT ( 'NONE',  ( -26.77998953358746803, 58.61463389606510788, -3.164065525718655181 ) ) ;
#10584 = CARTESIAN_POINT ( 'NONE',  ( -26.98076211353309972, 49.73333333333319928, -6.732050807568954909 ) ) ;
#10585 = DIRECTION ( 'NONE',  ( 0.000000000000000000, 0.000000000000000000, 1.000000000000000000 ) ) ;
#10586 =( NAMED_UNIT ( * ) SI_UNIT ( $, .STERADIAN. ) SOLID_ANGLE_UNIT ( ) );
#10587 = CARTESIAN_POINT ( 'NONE',  ( 25.78460820925620922, 50.00384911698630930, 2.500000000000000000 ) ) ;
#10588 = CARTESIAN_POINT ( 'NONE',  ( -3.500000000000002220, 28.55025253169416288, 14.04687500000000355 ) ) ;
#10589 = PLANE ( 'NONE',  #2412 ) ;
#10590 = EDGE_CURVE ( 'NONE', #10667, #1487, #5293, .T. ) ;
#10591 = EDGE_LOOP ( 'NONE', ( #766, #10678 ) ) ;
#10592 = CARTESIAN_POINT ( 'NONE',  ( 0.1217565302851089937, -3.710888496608915510, 0.5725525826504929139 ) ) ;
#10593 = CARTESIAN_POINT ( 'NONE',  ( -2.479565268636987785, 29.67421718125152452, 17.49702953738633937 ) ) ;
#10594 = CARTESIAN_POINT ( 'NONE',  ( 3.527408190673964494, 31.38357824266065776, 15.66968341526694175 ) ) ;
#10595 = CARTESIAN_POINT ( 'NONE',  ( 22.88317621546045189, 19.71992003298075957, 12.00579112326941988 ) ) ;
#10596 = CARTESIAN_POINT ( 'NONE',  ( -4.000000000000000000, -0.7890432684750890990, -0.04868663549882315533 ) ) ;
#10597 = CARTESIAN_POINT ( 'NONE',  ( 0.1404048886732821022, 4.699864953788070565, -3.686887068327037387 ) ) ;
#10598 = CARTESIAN_POINT ( 'NONE',  ( -27.60187600103308014, 52.28541666571061342, -5.935950539335252074 ) ) ;
#10599 = LINE ( 'NONE', #201, #5897 ) ;
#10600 = CARTESIAN_POINT ( 'NONE',  ( 25.00000000000000000, 0.000000000000000000, 0.000000000000000000 ) ) ;
#10601 = ORIENTED_EDGE ( 'NONE', *, *, #10284, .T. ) ;
#10602 = MECHANICAL_DESIGN_GEOMETRIC_PRESENTATION_REPRESENTATION (  '', ( #7393 ), #6152 ) ;
#10603 = SHAPE_REPRESENTATION ( 'caliper arm right', ( #308 ), #5109 ) ;
#10604 = FACE_OUTER_BOUND ( 'NONE', #6584, .T. ) ;
#10605 = ORIENTED_EDGE ( 'NONE', *, *, #2900, .F. ) ;
#10606 = LINE ( 'NONE', #5385, #7535 ) ;
#10607 = CARTESIAN_POINT ( 'NONE',  ( -25.98076211353310683, 50.59374999904395054, -6.871901078670399343 ) ) ;
#10608 = VECTOR ( 'NONE', #4798, 1000.000000000000000 ) ;
#10609 = TOROIDAL_SURFACE ( 'NONE', #7231, 3.369999999999997886, 0.1199999999999999956 ) ;
#10610 = EDGE_CURVE ( 'NONE', #8872, #998, #4213, .T. ) ;
#10611 = CARTESIAN_POINT ( 'NONE',  ( 18.76115673388714455, 17.03897527867736983, 11.01746215567925269 ) ) ;
#10612 = ORIENTED_EDGE ( 'NONE', *, *, #3701, .T. ) ;
#10613 = CYLINDRICAL_SURFACE ( 'NONE', #4053, 4.250000000000000000 ) ;
#10614 = EDGE_LOOP ( 'NONE', ( #6208, #5681 ) ) ;
#10615 = DIRECTION ( 'NONE',  ( -0.000000000000000000, 0.000000000000000000, 1.000000000000000000 ) ) ;
#10616 = EDGE_LOOP ( 'NONE', ( #4503, #10212, #9892 ) ) ;
#10617 = AXIS2_PLACEMENT_3D ( 'NONE', #8051, #1438, #8208 ) ;
#10618 = CARTESIAN_POINT ( 'NONE',  ( 1.767766952966372429, 31.76776695296637598, 13.50000000000000355 ) ) ;
#10619 = SHAPE_REPRESENTATION_RELATIONSHIP ( 'NONE' , 'NONE' ,  #5757, #9310 ) ;
#10620 = ORIENTED_EDGE ( 'NONE', *, *, #1460, .F. ) ;
#10621 = STYLED_ITEM ( 'NONE', ( #7818 ), #1846 ) ;
#10622 = CARTESIAN_POINT ( 'NONE',  ( 22.57450250028656669, 18.29201386669844709, 10.95195840513859231 ) ) ;
#10623 = ADVANCED_FACE ( 'NONE', ( #4518 ), #9840, .F. ) ;
#10624 = DIRECTION ( 'NONE',  ( 0.000000000000000000, 0.000000000000000000, -1.000000000000000000 ) ) ;
#10625 = EDGE_CURVE ( 'NONE', #1406, #3226, #9896, .T. ) ;
#10626 = CARTESIAN_POINT ( 'NONE',  ( 20.11906803080876571, 17.66537948065741759, 13.00425721518307576 ) ) ;
#10627 = AXIS2_PLACEMENT_3D ( 'NONE', #10638, #7341, #2243 ) ;
#10628 = CARTESIAN_POINT ( 'NONE',  ( -26.98076211353309972, 52.67916666475470322, -3.267949192431252037 ) ) ;
#10629 = ADVANCED_FACE ( 'NONE', ( #8060 ), #8118, .T. ) ;
#10630 = CARTESIAN_POINT ( 'NONE',  ( 3.999999999999999112, -0.7890432684750902093, -0.04868663549882291247 ) ) ;
#10631 = CARTESIAN_POINT ( 'NONE',  ( -25.98076211353324894, 14.99999999999984190, -2.500000000000000000 ) ) ;
#10632 = EDGE_LOOP ( 'NONE', ( #10576, #6329, #679, #10020 ) ) ;
#10633 = EDGE_LOOP ( 'NONE', ( #8827, #889 ) ) ;
#10634 = CARTESIAN_POINT ( 'NONE',  ( 19.29066956973784386, 17.16581860495888634, 12.00630190750973370 ) ) ;
#10635 = ADVANCED_FACE ( 'NONE', ( #1343 ), #10609, .F. ) ;
#10636 = B_SPLINE_CURVE_WITH_KNOTS ( 'NONE', 3,
 ( #6255, #2776, #9648, #2939 ),
 .UNSPECIFIED., .F., .F.,
 ( 4, 4 ),
 ( 2.380739282167226656E-07, 0.002044882221487536681 ),
 .UNSPECIFIED. ) ;
#10637 = DIRECTION ( 'NONE',  ( -0.000000000000000000, -0.000000000000000000, 1.000000000000000000 ) ) ;
#10638 = CARTESIAN_POINT ( 'NONE',  ( -25.71106610644865498, 0.000000000000000000, -5.000000000000000000 ) ) ;
#10639 = CARTESIAN_POINT ( 'NONE',  ( -25.36430081112252211, 57.20223309010732748, -6.905092627761828972 ) ) ;
#10640 = EDGE_CURVE ( 'NONE', #4773, #10561, #430, .T. ) ;
#10641 = EDGE_CURVE ( 'NONE', #10050, #4107, #6673, .T. ) ;
#10642 = CARTESIAN_POINT ( 'NONE',  ( 4.000000000000000000, 2.309401076758515803, -0.4999999999999995559 ) ) ;
#10643 = CARTESIAN_POINT ( 'NONE',  ( 3.500000000000007994, 29.93383077435482420, 16.84155841526694175 ) ) ;
#10644 = DIRECTION ( 'NONE',  ( 0.000000000000000000, -0.000000000000000000, -1.000000000000000000 ) ) ;
#10645 = ORIENTED_EDGE ( 'NONE', *, *, #9498, .F. ) ;
#10646 = CARTESIAN_POINT ( 'NONE',  ( 4.000000000000000000, 2.309401076758515803, -0.4999999999999995559 ) ) ;
#10647 = CARTESIAN_POINT ( 'NONE',  ( 0.06616922564517249694, 32.50000000000000711, 14.65405841526694353 ) ) ;
#10648 = DIRECTION ( 'NONE',  ( 1.156482317317871725E-16, -2.312964634635742464E-16, -1.000000000000000000 ) ) ;
#10649 = DIRECTION ( 'NONE',  ( -1.000000000000000000, -0.000000000000000000, -0.000000000000000000 ) ) ;
#10650 = LINE ( 'NONE', #3039, #5426 ) ;
#10651 = CARTESIAN_POINT ( 'NONE',  ( -26.98076211353309972, 51.13333333333319786, -6.732050807568954909 ) ) ;
#10652 = CARTESIAN_POINT ( 'NONE',  ( -25.98076211353311393, 50.76874999904394770, -6.871901078670400231 ) ) ;
#10653 = DIRECTION ( 'NONE',  ( -1.000000000000000000, 0.000000000000000000, 0.000000000000000000 ) ) ;
#10654 = CARTESIAN_POINT ( 'NONE',  ( -0.5636800770129166693, -4.293361309317430319, -3.531542292955206275 ) ) ;
#10655 = ORIENTED_EDGE ( 'NONE', *, *, #6338, .F. ) ;
#10656 = CARTESIAN_POINT ( 'NONE',  ( -24.98076211353313170, 54.19583333142136894, -3.267949192431250705 ) ) ;
#10657 = CARTESIAN_POINT ( 'NONE',  ( -31.74999999999995737, 0.000000000000000000, 0.000000000000000000 ) ) ;
#10658 = EDGE_CURVE ( 'NONE', #9804, #9319, #658, .T. ) ;
#10659 = ORIENTED_EDGE ( 'NONE', *, *, #10443, .T. ) ;
#10660 = FACE_OUTER_BOUND ( 'NONE', #3719, .T. ) ;
#10661 = CARTESIAN_POINT ( 'NONE',  ( 0.1388410611046147491, -3.710337782248049887, -0.5735064479039554408 ) ) ;
#10662 = CARTESIAN_POINT ( 'NONE',  ( 22.66010611969070965, 19.57566612754892432, 11.00732503135576401 ) ) ;
#10663 = VERTEX_POINT ( 'NONE', #3018 ) ;
#10664 = CARTESIAN_POINT ( 'NONE',  ( 34.66939513580730647, 4.803384628401708767, 2.499999999999999556 ) ) ;
#10665 = ORIENTED_EDGE ( 'NONE', *, *, #236, .T. ) ;
#10666 = FACE_OUTER_BOUND ( 'NONE', #4068, .T. ) ;
#10667 = VERTEX_POINT ( 'NONE', #4793 ) ;
#10668 = CARTESIAN_POINT ( 'NONE',  ( 25.98076211353311749, 53.49999999999983658, 12.14999999999999147 ) ) ;
#10669 = CIRCLE ( 'NONE', #9064, 0.5155456020628804703 ) ;
#10670 = ORIENTED_EDGE ( 'NONE', *, *, #5380, .T. ) ;
#10671 = CARTESIAN_POINT ( 'NONE',  ( 24.26768760078471487, 20.42249838054411271, 10.95195840513859586 ) ) ;
#10672 = CARTESIAN_POINT ( 'NONE',  ( 0.02937408083519552765, -0.6808742863896954933, -3.499999999999999556 ) ) ;
#10673 = CARTESIAN_POINT ( 'NONE',  ( 16.16243297953557700, 18.78731448874862053, 13.21853671947355302 ) ) ;
#10674 = TOROIDAL_SURFACE ( 'NONE', #9786, 5.384454397937118664, 0.5155456020628804703 ) ;
#10675 = CARTESIAN_POINT ( 'NONE',  ( -23.98076211353314235, 52.97083333142136041, -6.154700538379337615 ) ) ;
#10676 = DIRECTION ( 'NONE',  ( -1.000000000000000000, -0.000000000000000000, -0.000000000000000000 ) ) ;
#10677 = DIRECTION ( 'NONE',  ( 0.000000000000000000, -0.8660254037844391517, -0.4999999999999991673 ) ) ;
#10678 = ORIENTED_EDGE ( 'NONE', *, *, #3371, .T. ) ;
#10679 = ORIENTED_EDGE ( 'NONE', *, *, #10301, .F. ) ;
#10680 = CARTESIAN_POINT ( 'NONE',  ( 19.69775075566884226, 17.43975236193677603, 12.00579112326941988 ) ) ;
#10681 = DIRECTION ( 'NONE',  ( -0.000000000000000000, -0.000000000000000000, 1.000000000000000000 ) ) ;
#10682 = DIRECTION ( 'NONE',  ( -0.000000000000000000, -1.000000000000000000, -0.000000000000000000 ) ) ;
#10683 = AXIS2_PLACEMENT_3D ( 'NONE', #8708, #6149, #1315 ) ;
#10684 = CARTESIAN_POINT ( 'NONE',  ( -27.98076211353308551, 52.56249999808803608, -5.000000000000103029 ) ) ;
#10685 = FACE_OUTER_BOUND ( 'NONE', #5534, .T. ) ;
#10686 = CARTESIAN_POINT ( 'NONE',  ( 2.428085025993350410, 32.52166244231248271, 15.00219158473306535 ) ) ;
#10687 = CARTESIAN_POINT ( 'NONE',  ( 34.99999999999999289, 1.431146867680865853E-14, -12.49999999999999822 ) ) ;
#10688 = ADVANCED_FACE ( 'NONE', ( #1400 ), #1874, .F. ) ;
#10689 = ORIENTED_EDGE ( 'NONE', *, *, #4597, .T. ) ;
#10690 = ADVANCED_FACE ( 'NONE', ( #6551 ), #8950, .F. ) ;
#10691 = ORIENTED_EDGE ( 'NONE', *, *, #5633, .T. ) ;
#10692 = CARTESIAN_POINT ( 'NONE',  ( 1.720978244806812496, 28.18544433887406342, 15.43530841526694175 ) ) ;
#10693 = CIRCLE ( 'NONE', #9808, 3.499999999999999556 ) ;
#10694 = CARTESIAN_POINT ( 'NONE',  ( 29.50000000000000711, -3.999999999999989786, 7.850000000000005862 ) ) ;
#10695 = DIRECTION ( 'NONE',  ( 0.000000000000000000, 1.000000000000000000, 0.000000000000000000 ) ) ;
#10696 = CARTESIAN_POINT ( 'NONE',  ( -2.500000000000007550, 31.03553390593274131, 13.89062500000000355 ) ) ;
#10697 = CARTESIAN_POINT ( 'NONE',  ( 0.000000000000000000, 0.8865213383406715941, 1.535499999999999199 ) ) ;
#10698 = CARTESIAN_POINT ( 'NONE',  ( -25.98076211353311393, 50.94374999904395196, -3.128098921329806714 ) ) ;
#10699 = FACE_OUTER_BOUND ( 'NONE', #8971, .T. ) ;
#10700 = CARTESIAN_POINT ( 'NONE',  ( -4.140404888673278272, -2.228338276487456415, -3.686887068327035166 ) ) ;
#10701 = ORIENTED_EDGE ( 'NONE', *, *, #4819, .T. ) ;
#10702 = DIRECTION ( 'NONE',  ( 1.000000000000000000, 0.000000000000000000, 0.000000000000000000 ) ) ;
#10703 = DIRECTION ( 'NONE',  ( -4.312387734422005941E-17, 0.7071067811865500152, -0.7071067811865451302 ) ) ;
#10704 = CARTESIAN_POINT ( 'NONE',  ( -24.35964822603314772, 50.65208333237728056, -5.935950539335252074 ) ) ;
#10705 = CARTESIAN_POINT ( 'NONE',  ( -27.60187600103308725, 54.32708333237728482, -4.064049460664955760 ) ) ;
#10706 = CARTESIAN_POINT ( 'NONE',  ( 21.41951502703731691, 22.64547864373410135, 12.00579112326941988 ) ) ;
#10707 = CARTESIAN_POINT ( 'NONE',  ( -27.60187600103308014, 55.02708333237728056, -4.064049460664955760 ) ) ;
#10708 = EDGE_LOOP ( 'NONE', ( #6914, #8377 ) ) ;
#10709 = CARTESIAN_POINT ( 'NONE',  ( 0.1999999999999987899, 4.041334437186265510E-16, -3.299999999999999822 ) ) ;
#10710 = AXIS2_PLACEMENT_3D ( 'NONE', #4102, #9777, #2169 ) ;
#10712 = ORIENTED_EDGE ( 'NONE', *, *, #1537, .T. ) ;
#10711 = EDGE_CURVE ( 'NONE', #4045, #990, #2574, .T. ) ;
#10713 = CARTESIAN_POINT ( 'NONE',  ( -25.98076211353311393, 49.49999999999986500, -5.000000000000103029 ) ) ;
#10714 = ORIENTED_EDGE ( 'NONE', *, *, #3959, .F. ) ;
#10715 = DIRECTION ( 'NONE',  ( 0.000000000000000000, 0.000000000000000000, -1.000000000000000000 ) ) ;
#10716 = VERTEX_POINT ( 'NONE', #4228 ) ;
#10717 = CARTESIAN_POINT ( 'NONE',  ( 20.78941077755876776, 23.50360388977173187, 10.95195840513859231 ) ) ;
#10718 = DIRECTION ( 'NONE',  ( 0.000000000000000000, -1.000000000000000000, 0.000000000000000000 ) ) ;
#10719 = CARTESIAN_POINT ( 'NONE',  ( 20.55933174294505861, 16.75535677129292722, 12.94889058896590583 ) ) ;
#10720 = CARTESIAN_POINT ( 'NONE',  ( -27.98076211353308551, 53.32083333142136894, -3.845299461620869330 ) ) ;
#10721 = VECTOR ( 'NONE', #3652, 1000.000000000000000 ) ;
#10722 = CARTESIAN_POINT ( 'NONE',  ( -26.98076211353309972, 53.46666666666653356, -3.267949192431252037 ) ) ;
#10723 = DIRECTION ( 'NONE',  ( -0.000000000000000000, -0.000000000000000000, -1.000000000000000000 ) ) ;
#10724 = EDGE_LOOP ( 'NONE', ( #4171, #2567, #9935, #4888, #5483 ) ) ;
#10725 = CLOSED_SHELL ( 'NONE', ( #9651, #4932, #8692, #10623, #4866, #3759, #8891, #5826, #9132, #565, #8251, #4654, #23, #377, #5022, #6883, #8751, #6450, #8013, #6141, #10690, #8312, #4519, #5193, #7829, #1954, #9800, #3696, #4489, #6014, #4386, #1753, #6074, #6350, #2435, #2211, #4166, #1104, #1937 ) ) ;
#10726 = ORIENTED_EDGE ( 'NONE', *, *, #9464, .T. ) ;
#10727 = CARTESIAN_POINT ( 'NONE',  ( 20.23853826540680600, 19.71164639310234534, 12.00579112326941988 ) ) ;
#10728 = VECTOR ( 'NONE', #3548, 1000.000000000000000 ) ;
#10729 = CARTESIAN_POINT ( 'NONE',  ( -24.98076211353313170, 52.18333333333320212, -3.267949192431250705 ) ) ;
#10730 = AXIS2_PLACEMENT_3D ( 'NONE', #549, #664, #5627 ) ;
#10731 = CARTESIAN_POINT ( 'NONE',  ( 0.3126073911696528040, 2.020725942163738686, 3.499999999999999556 ) ) ;
#10733 = CARTESIAN_POINT ( 'NONE',  ( -26.59698951503823139, 57.20194332867976073, -3.094806908524387445 ) ) ;
#10732 = CIRCLE ( 'NONE', #4184, 2.149999999999992362 ) ;
#10734 = ADVANCED_FACE ( 'NONE', ( #3391 ), #759, .T. ) ;
#10735 = CARTESIAN_POINT ( 'NONE',  ( -2.500000000000003997, 29.93383077435482065, 12.97094158473306358 ) ) ;
#10736 = LINE ( 'NONE', #4700, #7199 ) ;
#10737 = EDGE_LOOP ( 'NONE', ( #10691, #4832, #6935, #4216 ) ) ;
#10738 = FACE_OUTER_BOUND ( 'NONE', #3994, .T. ) ;
#10739 = ORIENTED_EDGE ( 'NONE', *, *, #6670, .F. ) ;
#10740 = AXIS2_PLACEMENT_3D ( 'NONE', #8246, #1582, #3247 ) ;
#10741 = CARTESIAN_POINT ( 'NONE',  ( 0.06616922564517249694, 32.50000000000000711, 17.15405841526694175 ) ) ;
#10742 = CIRCLE ( 'NONE', #5256, 2.055000000000000160 ) ;
#10743 = CYLINDRICAL_SURFACE ( 'NONE', #1904, 1.999999999999971356 ) ;
#10744 = CARTESIAN_POINT ( 'NONE',  ( -25.44486372867087098, 52.06876073720499676, -3.000000000000133227 ) ) ;
#10745 = LINE ( 'NONE', #5593, #10207 ) ;
#10746 = EDGE_CURVE ( 'NONE', #8739, #3105, #3506, .T. ) ;
#10747 = DIRECTION ( 'NONE',  ( 0.000000000000000000, 0.000000000000000000, 1.000000000000000000 ) ) ;
#10748 = CARTESIAN_POINT ( 'NONE',  ( -24.35964822603314772, 49.77708333237728766, -5.935950539335252074 ) ) ;
#10749 = EDGE_CURVE ( 'NONE', #5575, #1944, #5887, .T. ) ;
#10750 = DIRECTION ( 'NONE',  ( 0.000000000000000000, 1.000000000000000000, 0.000000000000000000 ) ) ;
#10751 = CARTESIAN_POINT ( 'NONE',  ( -4.000000000000000000, 2.309401076758498483, -0.4999999999999927280 ) ) ;
#10752 = AXIS2_PLACEMENT_3D ( 'NONE', #361, #9033, #7255 ) ;
#10753 = ORIENTED_EDGE ( 'NONE', *, *, #8112, .F. ) ;
#10754 = B_SPLINE_CURVE_WITH_KNOTS ( 'NONE', 3,
 ( #8537, #2658, #4488, #7872 ),
 .UNSPECIFIED., .F., .F.,
 ( 4, 4 ),
 ( 2.380739282167534764E-07, 0.002044882221487497216 ),
 .UNSPECIFIED. ) ;
#10755 = CARTESIAN_POINT ( 'NONE',  ( -3.500000000000002665, 28.55025253169416288, 14.04687500000000355 ) ) ;
#10756 = DIRECTION ( 'NONE',  ( 0.000000000000000000, 0.000000000000000000, 1.000000000000000000 ) ) ;
#10757 = CARTESIAN_POINT ( 'NONE',  ( -25.98076211353310683, 50.76874999904394770, -6.871901078670399343 ) ) ;
#10758 = EDGE_CURVE ( 'NONE', #7385, #3226, #6172, .T. ) ;
#10759 = CARTESIAN_POINT ( 'NONE',  ( -24.35964822603314772, 53.27708333237728056, -5.935950539335252074 ) ) ;
#10760 = CARTESIAN_POINT ( 'NONE',  ( 21.90605485701305000, 18.97586566459109392, 12.00579112326941988 ) ) ;
#10761 =( LENGTH_UNIT ( ) NAMED_UNIT ( * ) SI_UNIT ( .MILLI., .METRE. ) );
#10762 = CARTESIAN_POINT ( 'NONE',  ( -24.35964822603314772, 54.56041666571061910, -4.064049460664953983 ) ) ;
#10763 = ORIENTED_EDGE ( 'NONE', *, *, #3083, .T. ) ;
#10764 = EDGE_CURVE ( 'NONE', #7545, #8989, #8471, .T. ) ;
#10765 = EDGE_CURVE ( 'NONE', #2956, #5318, #10073, .T. ) ;
#10766 = CARTESIAN_POINT ( 'NONE',  ( 34.64101615137754209, 5.000000000000000888, 2.500000000000000000 ) ) ;
#10767 = ADVANCED_BREP_SHAPE_REPRESENTATION ( '', ( #5578, #308 ), #6687 ) ;
#10768 = ORIENTED_EDGE ( 'NONE', *, *, #2908, .F. ) ;
#10769 = ORIENTED_EDGE ( 'NONE', *, *, #2542, .F. ) ;
#10770 = DIRECTION ( 'NONE',  ( -0.1561119869139967753, 0.9855205127846311530, -0.06616922564517428718 ) ) ;
#10771 = EDGE_LOOP ( 'NONE', ( #9592, #2168, #4148, #353, #9278 ) ) ;
#10772 = CARTESIAN_POINT ( 'NONE',  ( 1.567478505476134606E-15, 4.618802153517012066, -5.000000000000000000 ) ) ;
#10773 =( LENGTH_UNIT ( ) NAMED_UNIT ( * ) SI_UNIT ( .MILLI., .METRE. ) );
#10774 = EDGE_LOOP ( 'NONE', ( #9778, #5251, #4838, #216, #9667, #2157 ) ) ;
#10775 = CARTESIAN_POINT ( 'NONE',  ( 19.83233192245754140, 21.00689442486442360, 11.00732503135576401 ) ) ;
#10776 = AXIS2_PLACEMENT_3D ( 'NONE', #1724, #2500, #7497 ) ;
#10777 = LINE ( 'NONE', #820, #6119 ) ;
#10778 = CARTESIAN_POINT ( 'NONE',  ( 4.175648173966055587, -2.207990556236547608, -3.469390959564065291 ) ) ;
#10779 = CARTESIAN_POINT ( 'NONE',  ( 19.49929303312607942, 16.16195407633872350, 11.95465698723049108 ) ) ;
#10780 = CARTESIAN_POINT ( 'NONE',  ( -23.98076211353314235, 51.51249999808803182, -5.000000000000103029 ) ) ;
#10781 = AXIS2_PLACEMENT_3D ( 'NONE', #8561, #3398, #9445 ) ;
#10782 = PRESENTATION_LAYER_ASSIGNMENT (  '', '', ( #4233 ) ) ;
#10783 = CARTESIAN_POINT ( 'NONE',  ( 34.90224802882305255, 2.616310811731261676, -3.667896704194531843 ) ) ;
#10784 = CARTESIAN_POINT ( 'NONE',  ( 34.99999999999987210, -3.999999999999989786, -4.999999999999999112 ) ) ;
#10785 = ORIENTED_EDGE ( 'NONE', *, *, #7153, .F. ) ;
#10786 = CARTESIAN_POINT ( 'NONE',  ( 0.06616922564517314920, 33.50000000000000000, 17.15405841526694175 ) ) ;
#10787 = ORIENTED_EDGE ( 'NONE', *, *, #9399, .F. ) ;
#10788 = B_SPLINE_CURVE_WITH_KNOTS ( 'NONE', 3,
 ( #3579, #9353, #1749, #4303, #10351, #65, #6852, #1803, #6125, #2862, #2180, #1239 ),
 .UNSPECIFIED., .F., .F.,
 ( 4, 2, 2, 2, 2, 4 ),
 ( 0.003180596909393765097, 0.003379140308194210698, 0.003577683706994655866, 0.003974770504595546636, 0.004371857302196437839, 0.004768944099797328175 ),
 .UNSPECIFIED. ) ;
#10789 = EDGE_CURVE ( 'NONE', #7434, #7695, #9331, .T. ) ;
#10790 = CARTESIAN_POINT ( 'NONE',  ( 20.29953126043439227, 16.57463755921569515, 12.94889058896590583 ) ) ;
#10791 = CARTESIAN_POINT ( 'NONE',  ( -25.98076211353311393, 51.07499999999986784, -7.000000000000073719 ) ) ;
#10792 = AXIS2_PLACEMENT_3D ( 'NONE', #7675, #5125, #4285 ) ;
#10793 = DIRECTION ( 'NONE',  ( 0.000000000000000000, -0.4999999999999991118, 0.8660254037844391517 ) ) ;
#10794 = DIRECTION ( 'NONE',  ( 0.000000000000000000, 1.000000000000000000, 0.000000000000000000 ) ) ;
#10795 = CARTESIAN_POINT ( 'NONE',  ( -0.06616922564517661864, 33.50000000000000000, 15.15844158473306535 ) ) ;
#10796 = DIRECTION ( 'NONE',  ( 0.000000000000000000, 0.000000000000000000, 1.000000000000000000 ) ) ;
#10797 = ORIENTED_EDGE ( 'NONE', *, *, #429, .F. ) ;
#10798 = FACE_OUTER_BOUND ( 'NONE', #3619, .T. ) ;
#10799 = B_SPLINE_CURVE_WITH_KNOTS ( 'NONE', 3,
 ( #3068, #1404, #7390, #9057, #4845, #5573, #2179, #10783, #8954, #8219, #6554, #606, #9952, #2336, #5780, #1503, #8124, #4905 ),
 .UNSPECIFIED., .F., .F.,
 ( 4, 2, 2, 2, 2, 2, 2, 2, 4 ),
 ( 0.000000000000000000, 0.0005875687307069781158, 0.001175137461413956232, 0.001762706192120934131, 0.002350274922827913331, 0.002937843653534892747, 0.003525412384241871731, 0.004112981114948850714, 0.004700549845655830131 ),
 .UNSPECIFIED. ) ;
#10800 = ORIENTED_EDGE ( 'NONE', *, *, #9192, .T. ) ;
#10801 = CARTESIAN_POINT ( 'NONE',  ( -2.521662442312483599, 27.57191497400664204, 15.12280841526694353 ) ) ;
#10802 = CARTESIAN_POINT ( 'NONE',  ( 29.50000000000000711, 1.387778780781445676E-14, -12.50000000000000000 ) ) ;
#10803 = EDGE_CURVE ( 'NONE', #998, #5599, #5835, .T. ) ;
#10804 = CARTESIAN_POINT ( 'NONE',  ( 17.65010306112908722, 17.31038946799904465, 12.07741653513508417 ) ) ;
#10805 = FACE_OUTER_BOUND ( 'NONE', #10932, .T. ) ;
#10806 = LINE ( 'NONE', #9973, #6941 ) ;
#10807 = CARTESIAN_POINT ( 'NONE',  ( -25.98076211353311393, 54.61874999904394912, -3.128098921329806714 ) ) ;
#10808 = DIRECTION ( 'NONE',  ( -0.000000000000000000, -0.000000000000000000, -1.000000000000000000 ) ) ;
#10809 = PLANE ( 'NONE',  #2592 ) ;
#10810 = ORIENTED_EDGE ( 'NONE', *, *, #838, .T. ) ;
#10811 = CARTESIAN_POINT ( 'NONE',  ( -2.474873734152920335, 32.47487373415291501, 13.81250000000000355 ) ) ;
#10812 = CARTESIAN_POINT ( 'NONE',  ( 3.199999999999999734, -3.031088913245509886, 1.750000000000043077 ) ) ;
#10813 = EDGE_CURVE ( 'NONE', #7419, #1521, #5099, .T. ) ;
#10814 = ADVANCED_FACE ( 'NONE', ( #2557 ), #135, .T. ) ;
#10815 = LINE ( 'NONE', #6477, #2216 ) ;
#10816 = CARTESIAN_POINT ( 'NONE',  ( -27.60187600103308725, 52.22708333237728340, -4.064049460664955760 ) ) ;
#10817 = CARTESIAN_POINT ( 'NONE',  ( 23.04535143233503192, 19.92821688535955360, 12.00579112326941988 ) ) ;
#10818 = CARTESIAN_POINT ( 'NONE',  ( -25.98076211353311393, 51.42499999999986215, -2.690598923241634743 ) ) ;
#10819 = ORIENTED_EDGE ( 'NONE', *, *, #9822, .F. ) ;
#10820 = APPLICATION_CONTEXT ( 'automotive_design' ) ;
#10821 = CARTESIAN_POINT ( 'NONE',  ( 34.80692069235084318, 3.675807134350209004, 2.800930295893637734 ) ) ;
#10822 = ADVANCED_FACE ( 'NONE', ( #3335 ), #2621, .F. ) ;
#10823 = EDGE_LOOP ( 'NONE', ( #8507, #7810, #8795 ) ) ;
#10824 = VERTEX_POINT ( 'NONE', #8501 ) ;
#10825 = FACE_OUTER_BOUND ( 'NONE', #6245, .T. ) ;
#10827 = ORIENTED_EDGE ( 'NONE', *, *, #2276, .F. ) ;
#10826 = EDGE_CURVE ( 'NONE', #9873, #1738, #8386, .T. ) ;
#10828 = DIRECTION ( 'NONE',  ( -1.000000000000000000, -6.098637220230963674E-17, 0.000000000000000000 ) ) ;
#10829 = CARTESIAN_POINT ( 'NONE',  ( 38.99999999999992184, -3.999999999999885425, 10.00000000000032152 ) ) ;
#10830 = ORIENTED_EDGE ( 'NONE', *, *, #823, .F. ) ;
#10831 = CARTESIAN_POINT ( 'NONE',  ( 15.88045857259785087, 19.06928889570832197, 12.24278471274156388 ) ) ;
#10832 =( NAMED_UNIT ( * ) SI_UNIT ( $, .STERADIAN. ) SOLID_ANGLE_UNIT ( ) );
#10833 = DIRECTION ( 'NONE',  ( 0.000000000000000000, 0.000000000000000000, 1.000000000000000000 ) ) ;
#10834 = CARTESIAN_POINT ( 'NONE',  ( 0.3126073911691547025, -2.020725942164465661, -3.499999999999999556 ) ) ;
#10835 = CARTESIAN_POINT ( 'NONE',  ( 18.70477062293933557, 21.09978808922912208, 12.94889058896590583 ) ) ;
#10836 = CARTESIAN_POINT ( 'NONE',  ( -26.98076211353309972, 51.74583333142136610, -6.732050807568954909 ) ) ;
#10837 = CARTESIAN_POINT ( 'NONE',  ( 3.200000000000000178, 4.041451884327400101, -2.303506639521620593E-14 ) ) ;
#10838 = CARTESIAN_POINT ( 'NONE',  ( -26.51666049839535688, 51.30623925897106830, -3.000000000000134115 ) ) ;
#10839 = VERTEX_POINT ( 'NONE', #6721 ) ;
#10840 = CARTESIAN_POINT ( 'NONE',  ( 1.383578242660662871, 26.47259180932604039, 15.35718341526694530 ) ) ;
#10841 = EDGE_LOOP ( 'NONE', ( #8031, #8404, #849 ) ) ;
#10842 = CARTESIAN_POINT ( 'NONE',  ( 22.92515349615029407, 19.68371071013345741, 13.00425721518307753 ) ) ;
#10843 = AXIS2_PLACEMENT_3D ( 'NONE', #8641, #8582, #3640 ) ;
#10844 = DIRECTION ( 'NONE',  ( -1.000000000000000000, -0.000000000000000000, -0.000000000000000000 ) ) ;
#10845 = FACE_OUTER_BOUND ( 'NONE', #5134, .T. ) ;
#10846 = DIRECTION ( 'NONE',  ( 1.000000000000000000, -0.000000000000000000, -0.000000000000000000 ) ) ;
#10847 = CARTESIAN_POINT ( 'NONE',  ( 0.06616922564517943584, 27.49999999999998934, 13.28344158473306713 ) ) ;
#10848 = CARTESIAN_POINT ( 'NONE',  ( 16.53922696119707325, 18.41052050710911914, 11.17880707182957600 ) ) ;
#10849 = DIRECTION ( 'NONE',  ( 0.000000000000000000, 1.000000000000000000, 0.000000000000000000 ) ) ;
#10850 = CARTESIAN_POINT ( 'NONE',  ( -27.98076211353308551, 55.36249999808803324, -5.000000000000103029 ) ) ;
#10851 = ORIENTED_EDGE ( 'NONE', *, *, #3177, .T. ) ;
#10852 = ORIENTED_EDGE ( 'NONE', *, *, #6968, .T. ) ;
#10853 = ADVANCED_FACE ( 'NONE', ( #4282 ), #4573, .T. ) ;
#10854 = CARTESIAN_POINT ( 'NONE',  ( 0.000000000000000000, 0.000000000000000000, -3.499999999999999556 ) ) ;
#10855 = FACE_OUTER_BOUND ( 'NONE', #1688, .T. ) ;
#10856 = CARTESIAN_POINT ( 'NONE',  ( 25.49999999999999645, -3.999999999999983569, 10.00000000000000888 ) ) ;
#10857 = VECTOR ( 'NONE', #7992, 1000.000000000000000 ) ;
#10858 = CARTESIAN_POINT ( 'NONE',  ( -25.98076211353311038, 61.49999999999985789, -5.000000000000102141 ) ) ;
#10859 = CARTESIAN_POINT ( 'NONE',  ( 5.200000000000002842, 0.000000000000000000, 0.000000000000000000 ) ) ;
#10860 = CARTESIAN_POINT ( 'NONE',  ( -25.17020516978313083, 55.61041666571061626, -6.403925809002825709 ) ) ;
#10861 = DIRECTION ( 'NONE',  ( 0.000000000000000000, 1.000000000000000000, 0.000000000000000000 ) ) ;
#10862 = CARTESIAN_POINT ( 'NONE',  ( -31.74999999999995737, 0.000000000000000000, 0.000000000000000000 ) ) ;
#10863 = ORIENTED_EDGE ( 'NONE', *, *, #9123, .T. ) ;
#10864 = CARTESIAN_POINT ( 'NONE',  ( 24.49999999999999289, -6.767949192431108152, -4.999999999999992006 ) ) ;
#10865 = VECTOR ( 'NONE', #691, 1000.000000000000000 ) ;
#10866 = FACE_OUTER_BOUND ( 'NONE', #4056, .T. ) ;
#10867 = CARTESIAN_POINT ( 'NONE',  ( 29.50000000000000711, 2.000000000000001776, -12.50000000000000000 ) ) ;
#10868 = CARTESIAN_POINT ( 'NONE',  ( -27.60187600103308725, 51.58541666571061057, -5.935950539335252074 ) ) ;
#10869 = CARTESIAN_POINT ( 'NONE',  ( -24.35964822603314772, 53.86041666571061626, -4.064049460664953983 ) ) ;
#10870 = CARTESIAN_POINT ( 'NONE',  ( 21.05771646464872404, 22.57981893131178452, 12.00579112326941988 ) ) ;
#10871 = CARTESIAN_POINT ( 'NONE',  ( -24.98076211353313170, 52.88333333333319786, -3.267949192431250705 ) ) ;
#10872 = EDGE_LOOP ( 'NONE', ( #8635, #66, #156, #10234 ) ) ;
#10873 = DIRECTION ( 'NONE',  ( 0.000000000000000000, 0.000000000000000000, 1.000000000000000000 ) ) ;
#10874 = ORIENTED_EDGE ( 'NONE', *, *, #632, .T. ) ;
#10875 = VERTEX_POINT ( 'NONE', #7976 ) ;
#10876 = DIRECTION ( 'NONE',  ( -0.000000000000000000, -0.000000000000000000, -1.000000000000000000 ) ) ;
#10877 = VERTEX_POINT ( 'NONE', #2923 ) ;
#10878 = DIRECTION ( 'NONE',  ( -1.000000000000000000, -0.000000000000000000, -0.000000000000000000 ) ) ;
#10879 = VERTEX_POINT ( 'NONE', #4485 ) ;
#10880 = CARTESIAN_POINT ( 'NONE',  ( 17.59356678224322934, 17.35619608210146581, 12.08212522340233264 ) ) ;
#10881 = FILL_AREA_STYLE_COLOUR ( '', #10971 ) ;
#10882 = DIRECTION ( 'NONE',  ( 0.000000000000000000, 0.000000000000000000, 1.000000000000000000 ) ) ;
#10883 = CARTESIAN_POINT ( 'NONE',  ( -27.60187600103308014, 50.18541666571061199, -5.935950539335252074 ) ) ;
#10884 = EDGE_CURVE ( 'NONE', #4463, #4583, #1978, .T. ) ;
#10885 = CARTESIAN_POINT ( 'NONE',  ( 16.03488360227938969, 17.50065030365295016, 12.16198771834549497 ) ) ;
#10886 = AXIS2_PLACEMENT_3D ( 'NONE', #3554, #4613, #2109 ) ;
#10887 = CARTESIAN_POINT ( 'NONE',  ( -25.98076211353311393, 50.41874999904393917, -3.128098921329806714 ) ) ;
#10888 = CARTESIAN_POINT ( 'NONE',  ( 24.99999259214812142, 30.01924558493218598, -2.500000000000000000 ) ) ;
#10889 = ORIENTED_EDGE ( 'NONE', *, *, #4850, .F. ) ;
#10890 = CARTESIAN_POINT ( 'NONE',  ( 2.000000000000000000, -0.8865213383406694847, 1.535500000000001419 ) ) ;
#10891 = PRODUCT_DEFINITION_CONTEXT ( 'detailed design', #2888, 'design' ) ;
#10892 = ORIENTED_EDGE ( 'NONE', *, *, #1324, .F. ) ;
#10893 = CARTESIAN_POINT ( 'NONE',  ( -1.383578242660661983, 33.52740819067396671, 14.73218341526694175 ) ) ;
#10894 = ORIENTED_EDGE ( 'NONE', *, *, #409, .F. ) ;
#10895 = CARTESIAN_POINT ( 'NONE',  ( 16.70557116688603472, 16.82996273904517182, 13.10128505860060066 ) ) ;
#10896 = AXIS2_PLACEMENT_3D ( 'NONE', #7383, #10828, #3940 ) ;
#10897 = EDGE_CURVE ( 'NONE', #1093, #6429, #6876, .T. ) ;
#10898 = CARTESIAN_POINT ( 'NONE',  ( -24.98076211353213694, 57.99999999999985789, -6.732050807568384698 ) ) ;
#10899 = DIRECTION ( 'NONE',  ( 0.000000000000000000, 0.000000000000000000, -1.000000000000000000 ) ) ;
#10900 = CARTESIAN_POINT ( 'NONE',  ( 34.99999999999999289, -7.999999999999996447, -12.49999999999999822 ) ) ;
#10901 = CARTESIAN_POINT ( 'NONE',  ( 2.500000000000006661, 30.06616922564517580, 13.59594158473306358 ) ) ;
#10902 = DIRECTION ( 'NONE',  ( 4.891728712884731355E-16, -0.7071067811865489050, -0.7071067811865462405 ) ) ;
#10903 = AXIS2_PLACEMENT_3D ( 'NONE', #2945, #6260, #1214 ) ;
#10904 = VERTEX_POINT ( 'NONE', #3748 ) ;
#10905 = DIRECTION ( 'NONE',  ( -1.000000000000000000, 0.000000000000000000, 0.000000000000000000 ) ) ;
#10906 = EDGE_CURVE ( 'NONE', #10456, #3988, #3801, .T. ) ;
#10907 = VERTEX_POINT ( 'NONE', #10420 ) ;
#10908 = ORIENTED_EDGE ( 'NONE', *, *, #5148, .T. ) ;
#10909 = DIRECTION ( 'NONE',  ( 0.000000000000000000, 0.000000000000000000, 1.000000000000000000 ) ) ;
#10910 = CARTESIAN_POINT ( 'NONE',  ( -25.98076211353311393, 54.48749999808803324, -7.000000000000072831 ) ) ;
#10911 = AXIS2_PLACEMENT_3D ( 'NONE', #7333, #5679, #9844 ) ;
#10912 = CARTESIAN_POINT ( 'NONE',  ( 34.76713615931383572, 4.034733667027951221, -2.652855901285303908 ) ) ;
#10913 = AXIS2_PLACEMENT_3D ( 'NONE', #4706, #8242, #6412 ) ;
#10914 = CIRCLE ( 'NONE', #780, 34.99999999999999289 ) ;
#10915 = DIRECTION ( 'NONE',  ( 0.000000000000000000, 0.000000000000000000, -1.000000000000000000 ) ) ;
#10916 = CYLINDRICAL_SURFACE ( 'NONE', #7288, 2.149999999999992362 ) ;
#10917 = CARTESIAN_POINT ( 'NONE',  ( -24.35964822603314772, 51.17708333237728624, -5.935950539335252074 ) ) ;
#10918 = EDGE_CURVE ( 'NONE', #4777, #8327, #8286, .T. ) ;
#10919 = PLANE ( 'NONE',  #5998 ) ;
#10920 = DIRECTION ( 'NONE',  ( 0.000000000000000000, 0.000000000000000000, -1.000000000000000000 ) ) ;
#10921 = EDGE_LOOP ( 'NONE', ( #987, #2792, #4117, #3986, #4611 ) ) ;
#10922 = AXIS2_PLACEMENT_3D ( 'NONE', #1701, #5752, #8479 ) ;
#10923 = DIRECTION ( 'NONE',  ( 0.000000000000000000, 0.000000000000000000, -1.000000000000000000 ) ) ;
#10924 = CARTESIAN_POINT ( 'NONE',  ( -26.51666049839535688, 53.90626073911682425, -7.000000000000071942 ) ) ;
#10925 = CARTESIAN_POINT ( 'NONE',  ( -27.60187600103308725, 53.80208333237728624, -4.064049460664955760 ) ) ;
#10926 = CARTESIAN_POINT ( 'NONE',  ( -25.17020516978313083, 54.73541666571062336, -6.403925809002825709 ) ) ;
#10927 = CIRCLE ( 'NONE', #992, 2.149999999999994582 ) ;
#10928 = CARTESIAN_POINT ( 'NONE',  ( 15.88045857259785087, 19.06928889570832197, 12.24278471274156388 ) ) ;
#10929 = CARTESIAN_POINT ( 'NONE',  ( -27.98076211353308551, 52.00833333333319786, -3.845299461620869330 ) ) ;
#10930 = ORIENTED_EDGE ( 'NONE', *, *, #3987, .T. ) ;
#10931 = PLANE ( 'NONE',  #7583 ) ;
#10932 = EDGE_LOOP ( 'NONE', ( #1544, #7681, #10259, #1210 ) ) ;
#10933 = EDGE_LOOP ( 'NONE', ( #6979, #6990, #9166, #4319 ) ) ;
#10934 = CARTESIAN_POINT ( 'NONE',  ( 29.50000000000000711, 5.000000000000001776, -5.500000000000000000 ) ) ;
#10935 = VERTEX_POINT ( 'NONE', #7869 ) ;
#10936 = FACE_OUTER_BOUND ( 'NONE', #5895, .T. ) ;
#10937 = DIRECTION ( 'NONE',  ( 0.000000000000000000, 0.000000000000000000, 1.000000000000000000 ) ) ;
#10938 = ORIENTED_EDGE ( 'NONE', *, *, #9812, .F. ) ;
#10939 = VECTOR ( 'NONE', #8408, 1000.000000000000000 ) ;
#10940 = CARTESIAN_POINT ( 'NONE',  ( 18.10462311893278553, 17.05669763433401087, 12.04589798090090902 ) ) ;
#10941 = EDGE_CURVE ( 'NONE', #8989, #750, #10476, .T. ) ;
#10942 = DIRECTION ( 'NONE',  ( -1.000000000000000000, -0.000000000000000000, -0.000000000000000000 ) ) ;
#10943 = CARTESIAN_POINT ( 'NONE',  ( 18.64799062861727563, 15.97503555906617123, 11.97707131907271005 ) ) ;
#10944 = FACE_OUTER_BOUND ( 'NONE', #4346, .T. ) ;
#10945 = B_SPLINE_CURVE_WITH_KNOTS ( 'NONE', 3,
 ( #1768, #1819, #5103, #976, #2485 ),
 .UNSPECIFIED., .F., .F.,
 ( 4, 1, 4 ),
 ( 0.000000000000000000, 0.002309401076758506657, 0.004618802153517013315 ),
 .UNSPECIFIED. ) ;
#10946 = CARTESIAN_POINT ( 'NONE',  ( -26.98076211353309972, 54.77916666475469754, -3.267949192431252037 ) ) ;
#10947 = FACE_OUTER_BOUND ( 'NONE', #8066, .T. ) ;
#10948 = ORIENTED_EDGE ( 'NONE', *, *, #8584, .T. ) ;
#10949 = CARTESIAN_POINT ( 'NONE',  ( 34.99999999999999289, -17.99999999999998579, 7.500000000000053291 ) ) ;
#10950 = ORIENTED_EDGE ( 'NONE', *, *, #8581, .T. ) ;
#10951 = AXIS2_PLACEMENT_3D ( 'NONE', #5484, #2873, #9583 ) ;
#10952 = CARTESIAN_POINT ( 'NONE',  ( 2.474873734152918558, 32.47487373415292211, 14.75000000000000355 ) ) ;
#10953 = PRODUCT_RELATED_PRODUCT_CATEGORY ( 'part', '', ( #7680 ) ) ;
#10954 = ORIENTED_EDGE ( 'NONE', *, *, #572, .F. ) ;
#10955 = ADVANCED_FACE ( 'NONE', ( #6357 ), #1075, .T. ) ;
#10956 = CARTESIAN_POINT ( 'NONE',  ( 17.31044041986821469, 16.31370680995936695, 13.04945978079559765 ) ) ;
#10957 = EDGE_CURVE ( 'NONE', #3329, #3105, #2869, .T. ) ;
#10958 = DIRECTION ( 'NONE',  ( 0.000000000000000000, 1.000000000000000000, -9.783878858594328898E-16 ) ) ;
#10959 = AXIS2_PLACEMENT_3D ( 'NONE', #9930, #4878, #2366 ) ;
#10960 = VECTOR ( 'NONE', #9567, 1000.000000000000000 ) ;
#10961 = CARTESIAN_POINT ( 'NONE',  ( 24.49999999999999289, -3.999999999999986233, -4.999999999999992006 ) ) ;
#10962 = CARTESIAN_POINT ( 'NONE',  ( -25.98076211353311749, 56.99999999999886313, -3.000000000000122569 ) ) ;
#10963 = CARTESIAN_POINT ( 'NONE',  ( 1.720978244806805169, 31.81455566112594013, 15.00219158473306535 ) ) ;
#10964 = FACE_OUTER_BOUND ( 'NONE', #4809, .T. ) ;
#10965 = CARTESIAN_POINT ( 'NONE',  ( 29.50000000000000711, 2.000000000000001776, -2.500000000000000000 ) ) ;
#10966 = FACE_OUTER_BOUND ( 'NONE', #2437, .T. ) ;
#10967 = ORIENTED_EDGE ( 'NONE', *, *, #5871, .T. ) ;
#10968 = EDGE_CURVE ( 'NONE', #4272, #7462, #8806, .T. ) ;
#10969 = ORIENTED_EDGE ( 'NONE', *, *, #3089, .F. ) ;
#10970 = VECTOR ( 'NONE', #7748, 1000.000000000000114 ) ;
#10971 = COLOUR_RGB ( '', 0.31764706, 0.68627451, 0.89019608) ;
#10972 = DIRECTION ( 'NONE',  ( 0.000000000000000000, 0.000000000000000000, 1.000000000000000000 ) ) ;
#10973 = CARTESIAN_POINT ( 'NONE',  ( -1.917253639661504005E-15, 3.375361811986492988, -1.153701847711665618 ) ) ;
#10974 = AXIS2_PLACEMENT_3D ( 'NONE', #9416, #3310, #2656 ) ;
#10975 = CARTESIAN_POINT ( 'NONE',  ( 23.33980466280999977, 20.94445964013513617, 12.00579112326902909 ) ) ;
#10976 = APPLICATION_CONTEXT ( 'automotive_design' ) ;
#10977 = CARTESIAN_POINT ( 'NONE',  ( 29.49999999999999645, -3.999999999999986233, -3.349999999999996980 ) ) ;
#10978 = CARTESIAN_POINT ( 'NONE',  ( 34.86952523334976917, 3.022518564432433941, 3.235504471074991617 ) ) ;
#10979 = CARTESIAN_POINT ( 'NONE',  ( -25.17020516978313083, 53.33541666571061768, -6.403925809002825709 ) ) ;
#10980 = CARTESIAN_POINT ( 'NONE',  ( 2.000000000000000000, 2.065682573263594481E-15, 1.535500000000000309 ) ) ;
#10981 = DIRECTION ( 'NONE',  ( -0.000000000000000000, 0.000000000000000000, -1.000000000000000000 ) ) ;
#10982 = DIRECTION ( 'NONE',  ( 0.000000000000000000, 0.000000000000000000, 1.000000000000000000 ) ) ;
#10983 = VERTEX_POINT ( 'NONE', #7034 ) ;
#10984 = CARTESIAN_POINT ( 'NONE',  ( -26.98076211353309972, 50.66666666666652930, -3.267949192431252037 ) ) ;
#10985 = CARTESIAN_POINT ( 'NONE',  ( 34.99999999999987210, -9.999999999999998224, -12.50000000000000000 ) ) ;
#10986 = CARTESIAN_POINT ( 'NONE',  ( -27.60187600103308725, 54.50208333237726777, -4.064049460664955760 ) ) ;
#10987 = CARTESIAN_POINT ( 'NONE',  ( -26.79131905728310059, 55.55208333237728624, -6.403925809002825709 ) ) ;
#10988 = DIRECTION ( 'NONE',  ( -1.000000000000000000, -0.000000000000000000, -0.000000000000000000 ) ) ;
#10989 = CARTESIAN_POINT ( 'NONE',  ( -26.98076211353309972, 51.36666666666653214, -3.267949192431252037 ) ) ;
#10990 = EDGE_CURVE ( 'NONE', #6272, #3329, #7399, .T. ) ;
#10991 = ORIENTED_EDGE ( 'NONE', *, *, #7977, .F. ) ;
#10992 = VERTEX_POINT ( 'NONE', #2818 ) ;
#10993 = ORIENTED_EDGE ( 'NONE', *, *, #2144, .F. ) ;
#10994 = FACE_OUTER_BOUND ( 'NONE', #2374, .T. ) ;
#10995 = ORIENTED_EDGE ( 'NONE', *, *, #7443, .F. ) ;
#10996 = DIRECTION ( 'NONE',  ( 0.000000000000000000, 0.000000000000000000, -1.000000000000000000 ) ) ;
#10997 = VERTEX_POINT ( 'NONE', #4592 ) ;
#10998 = NEXT_ASSEMBLY_USAGE_OCCURRENCE ( 'NAUO1', ' ', ' ', #10140, #2815, $ ) ;
#10999 = NEXT_ASSEMBLY_USAGE_OCCURRENCE ( 'NAUO2', ' ', ' ', #10140, #1375, $ ) ;
#11000 = NEXT_ASSEMBLY_USAGE_OCCURRENCE ( 'NAUO3', ' ', ' ', #10140, #7765, $ ) ;
#11001 = NEXT_ASSEMBLY_USAGE_OCCURRENCE ( 'NAUO4', ' ', ' ', #10140, #8571, $ ) ;
#11002 = NEXT_ASSEMBLY_USAGE_OCCURRENCE ( 'NAUO5', ' ', ' ', #10140, #8986, $ ) ;
#11003 = NEXT_ASSEMBLY_USAGE_OCCURRENCE ( 'NAUO6', ' ', ' ', #10140, #7765, $ ) ;
#11004 = NEXT_ASSEMBLY_USAGE_OCCURRENCE ( 'NAUO7', ' ', ' ', #10140, #6528, $ ) ;
#11005 = NEXT_ASSEMBLY_USAGE_OCCURRENCE ( 'NAUO8', ' ', ' ', #10140, #6528, $ ) ;
#11006 = NEXT_ASSEMBLY_USAGE_OCCURRENCE ( 'NAUO9', ' ', ' ', #10140, #6528, $ ) ;
#11007 = NEXT_ASSEMBLY_USAGE_OCCURRENCE ( 'NAUO10', ' ', ' ', #10140, #6528, $ ) ;
#11008 = NEXT_ASSEMBLY_USAGE_OCCURRENCE ( 'NAUO11', ' ', ' ', #10140, #9799, $ ) ;
#11009 = NEXT_ASSEMBLY_USAGE_OCCURRENCE ( 'NAUO12', ' ', ' ', #10140, #6396, $ ) ;
#11010 = NEXT_ASSEMBLY_USAGE_OCCURRENCE ( 'NAUO13', ' ', ' ', #10140, #3420, $ ) ;
ENDSEC;
END-ISO-10303-21;
